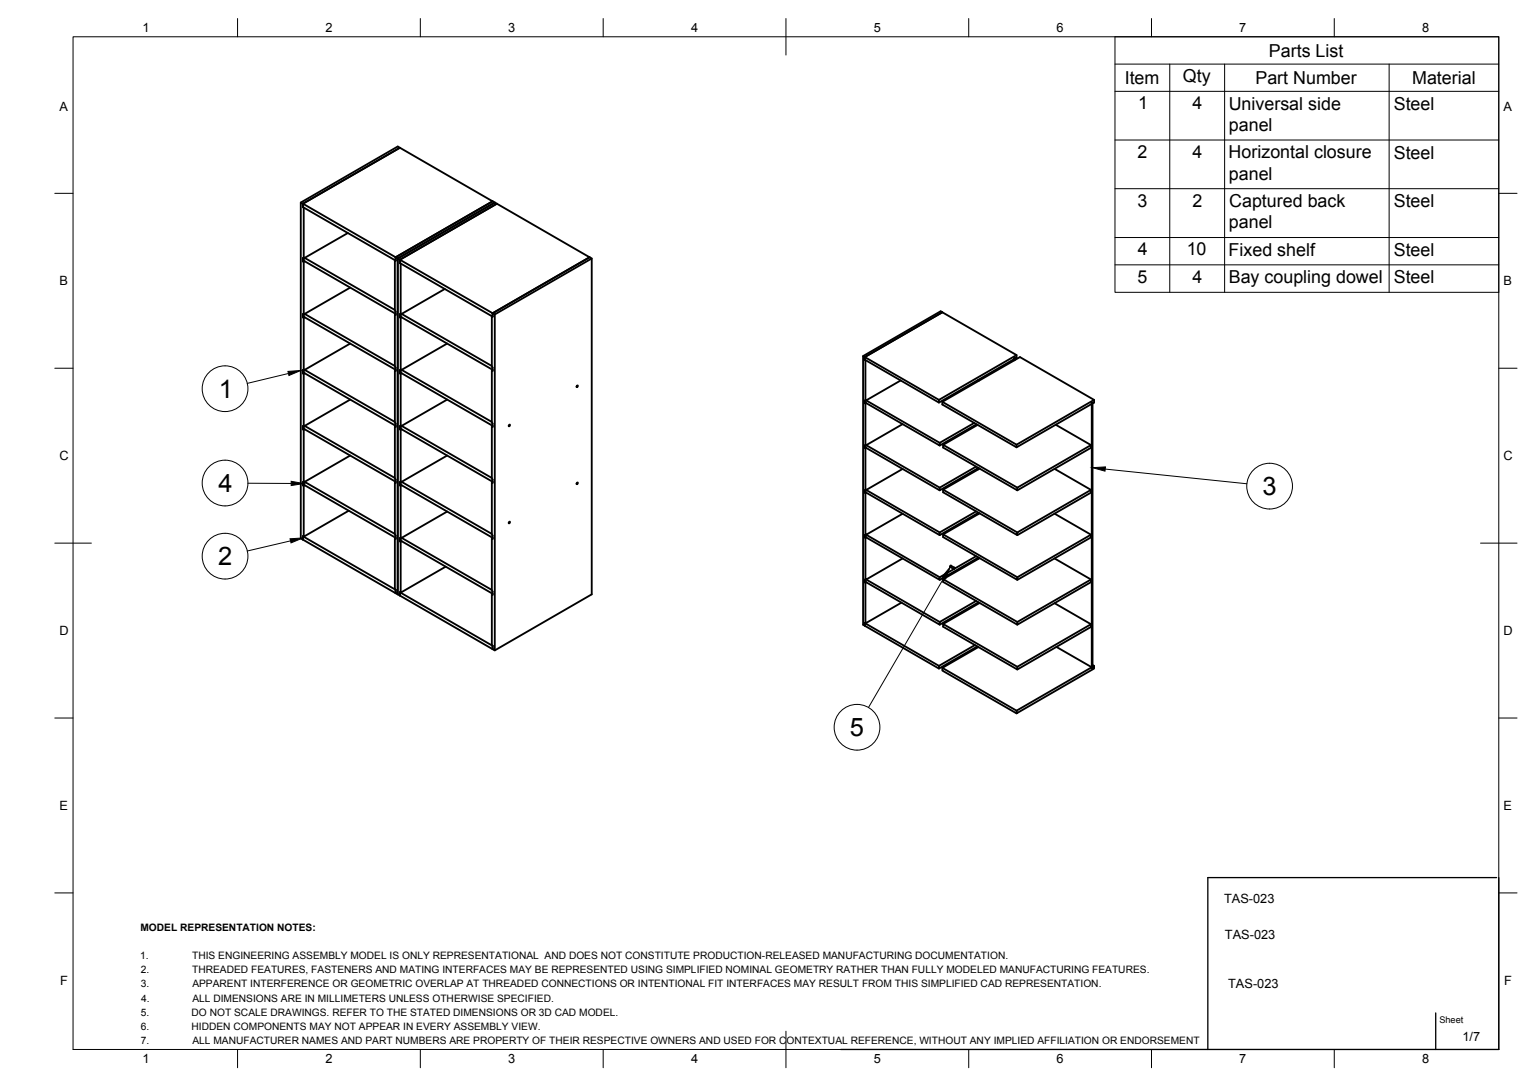
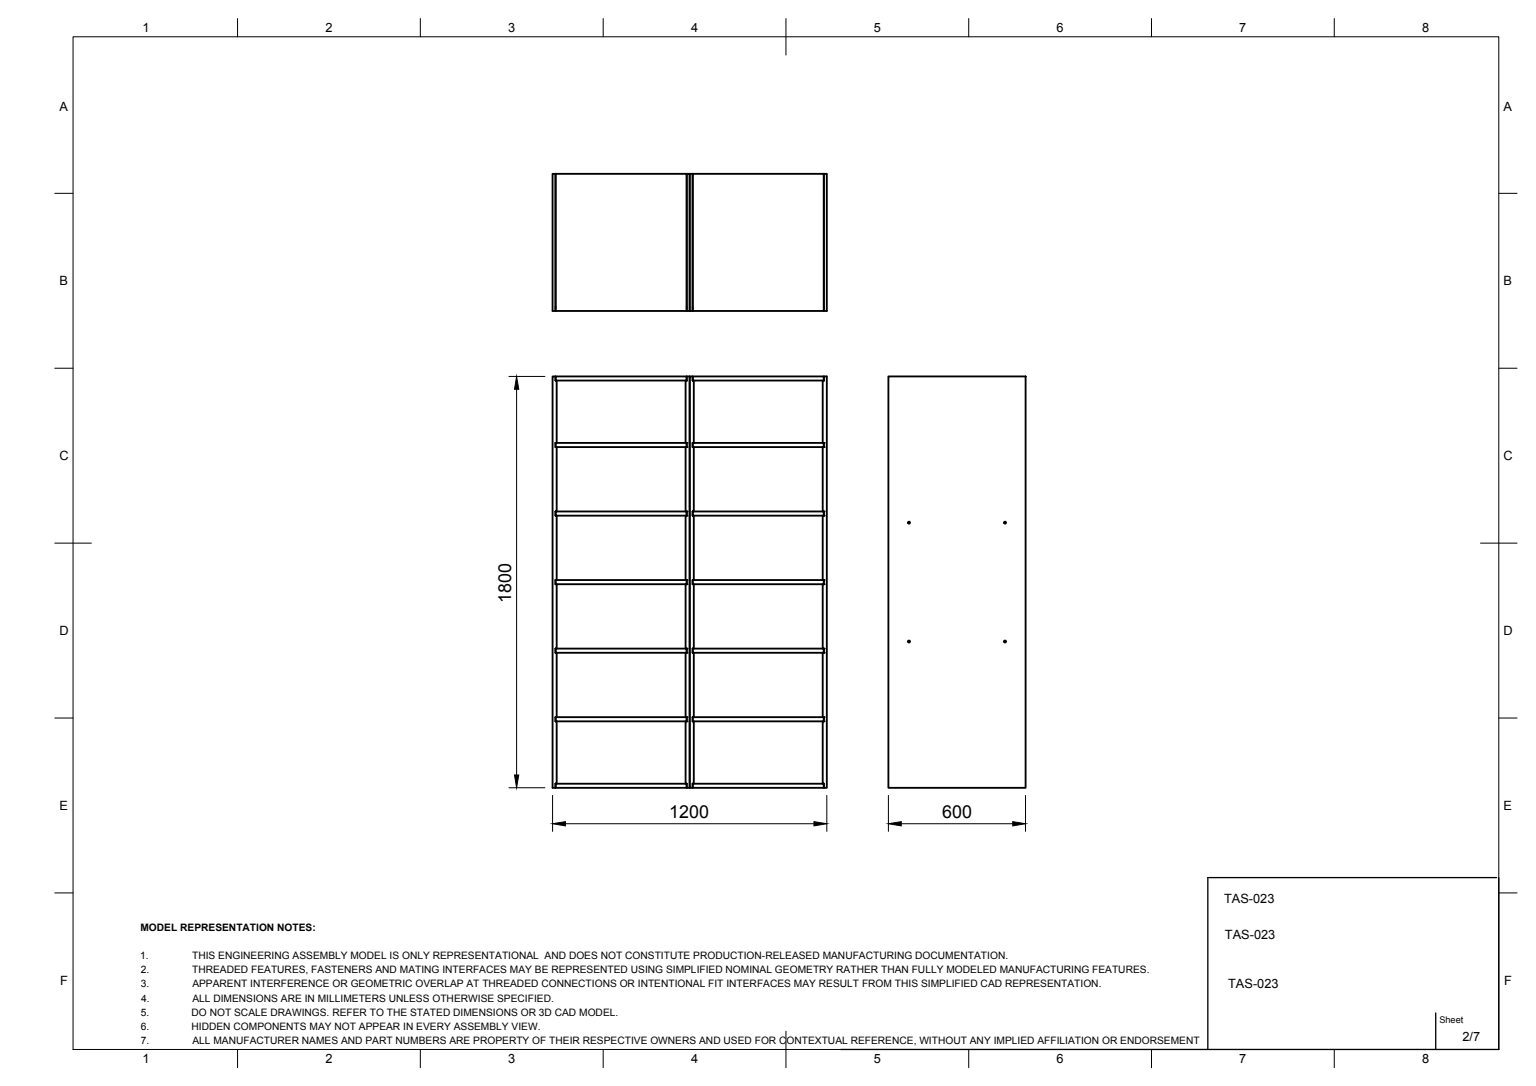
ISO-10303-21;
HEADER;
/* Generated by software containing ST-Developer
 * from STEP Tools, Inc. (www.steptools.com) 
 */

FILE_DESCRIPTION(
/* description */ (''),
/* implementation_level */ '2;1');

FILE_NAME(
/* name */ 'TAS-023.step',
/* time_stamp */ '2026-11-15T17:51:54-08:00',
/* author */ (''),
/* organization */ (''),
/* preprocessor_version */ 'ST-DEVELOPER v20.2',
/* originating_system */ 'Autodesk Translation Framework v15.17.0.0',
/* authorisation */ '');

FILE_SCHEMA (('AUTOMOTIVE_DESIGN { 1 0 10303 214 3 1 1 }'));
ENDSEC;

DATA;
#10=MECHANICAL_DESIGN_GEOMETRIC_PRESENTATION_REPRESENTATION('',(#117,#118,
#119,#120,#121),#2860);
#11=ITEM_DEFINED_TRANSFORMATION($,$,#1776,#1878);
#12=ITEM_DEFINED_TRANSFORMATION($,$,#1847,#1879);
#13=ITEM_DEFINED_TRANSFORMATION($,$,#1858,#1880);
#14=ITEM_DEFINED_TRANSFORMATION($,$,#1865,#1881);
#15=ITEM_DEFINED_TRANSFORMATION($,$,#1872,#1882);
#16=ITEM_DEFINED_TRANSFORMATION($,$,#1776,#1883);
#17=ITEM_DEFINED_TRANSFORMATION($,$,#1847,#1884);
#18=ITEM_DEFINED_TRANSFORMATION($,$,#1865,#1885);
#19=ITEM_DEFINED_TRANSFORMATION($,$,#1865,#1886);
#20=ITEM_DEFINED_TRANSFORMATION($,$,#1865,#1887);
#21=ITEM_DEFINED_TRANSFORMATION($,$,#1865,#1888);
#22=ITEM_DEFINED_TRANSFORMATION($,$,#1776,#1889);
#23=ITEM_DEFINED_TRANSFORMATION($,$,#1776,#1890);
#24=ITEM_DEFINED_TRANSFORMATION($,$,#1847,#1891);
#25=ITEM_DEFINED_TRANSFORMATION($,$,#1847,#1892);
#26=ITEM_DEFINED_TRANSFORMATION($,$,#1858,#1893);
#27=ITEM_DEFINED_TRANSFORMATION($,$,#1865,#1894);
#28=ITEM_DEFINED_TRANSFORMATION($,$,#1865,#1895);
#29=ITEM_DEFINED_TRANSFORMATION($,$,#1865,#1896);
#30=ITEM_DEFINED_TRANSFORMATION($,$,#1865,#1897);
#31=ITEM_DEFINED_TRANSFORMATION($,$,#1865,#1898);
#32=ITEM_DEFINED_TRANSFORMATION($,$,#1872,#1899);
#33=ITEM_DEFINED_TRANSFORMATION($,$,#1872,#1900);
#34=ITEM_DEFINED_TRANSFORMATION($,$,#1872,#1901);
#35=(
REPRESENTATION_RELATIONSHIP($,$,#2902,#2901)
REPRESENTATION_RELATIONSHIP_WITH_TRANSFORMATION(#11)
SHAPE_REPRESENTATION_RELATIONSHIP()
);
#36=(
REPRESENTATION_RELATIONSHIP($,$,#2903,#2901)
REPRESENTATION_RELATIONSHIP_WITH_TRANSFORMATION(#12)
SHAPE_REPRESENTATION_RELATIONSHIP()
);
#37=(
REPRESENTATION_RELATIONSHIP($,$,#2904,#2901)
REPRESENTATION_RELATIONSHIP_WITH_TRANSFORMATION(#13)
SHAPE_REPRESENTATION_RELATIONSHIP()
);
#38=(
REPRESENTATION_RELATIONSHIP($,$,#2905,#2901)
REPRESENTATION_RELATIONSHIP_WITH_TRANSFORMATION(#14)
SHAPE_REPRESENTATION_RELATIONSHIP()
);
#39=(
REPRESENTATION_RELATIONSHIP($,$,#2906,#2901)
REPRESENTATION_RELATIONSHIP_WITH_TRANSFORMATION(#15)
SHAPE_REPRESENTATION_RELATIONSHIP()
);
#40=(
REPRESENTATION_RELATIONSHIP($,$,#2902,#2901)
REPRESENTATION_RELATIONSHIP_WITH_TRANSFORMATION(#16)
SHAPE_REPRESENTATION_RELATIONSHIP()
);
#41=(
REPRESENTATION_RELATIONSHIP($,$,#2903,#2901)
REPRESENTATION_RELATIONSHIP_WITH_TRANSFORMATION(#17)
SHAPE_REPRESENTATION_RELATIONSHIP()
);
#42=(
REPRESENTATION_RELATIONSHIP($,$,#2905,#2901)
REPRESENTATION_RELATIONSHIP_WITH_TRANSFORMATION(#18)
SHAPE_REPRESENTATION_RELATIONSHIP()
);
#43=(
REPRESENTATION_RELATIONSHIP($,$,#2905,#2901)
REPRESENTATION_RELATIONSHIP_WITH_TRANSFORMATION(#19)
SHAPE_REPRESENTATION_RELATIONSHIP()
);
#44=(
REPRESENTATION_RELATIONSHIP($,$,#2905,#2901)
REPRESENTATION_RELATIONSHIP_WITH_TRANSFORMATION(#20)
SHAPE_REPRESENTATION_RELATIONSHIP()
);
#45=(
REPRESENTATION_RELATIONSHIP($,$,#2905,#2901)
REPRESENTATION_RELATIONSHIP_WITH_TRANSFORMATION(#21)
SHAPE_REPRESENTATION_RELATIONSHIP()
);
#46=(
REPRESENTATION_RELATIONSHIP($,$,#2902,#2901)
REPRESENTATION_RELATIONSHIP_WITH_TRANSFORMATION(#22)
SHAPE_REPRESENTATION_RELATIONSHIP()
);
#47=(
REPRESENTATION_RELATIONSHIP($,$,#2902,#2901)
REPRESENTATION_RELATIONSHIP_WITH_TRANSFORMATION(#23)
SHAPE_REPRESENTATION_RELATIONSHIP()
);
#48=(
REPRESENTATION_RELATIONSHIP($,$,#2903,#2901)
REPRESENTATION_RELATIONSHIP_WITH_TRANSFORMATION(#24)
SHAPE_REPRESENTATION_RELATIONSHIP()
);
#49=(
REPRESENTATION_RELATIONSHIP($,$,#2903,#2901)
REPRESENTATION_RELATIONSHIP_WITH_TRANSFORMATION(#25)
SHAPE_REPRESENTATION_RELATIONSHIP()
);
#50=(
REPRESENTATION_RELATIONSHIP($,$,#2904,#2901)
REPRESENTATION_RELATIONSHIP_WITH_TRANSFORMATION(#26)
SHAPE_REPRESENTATION_RELATIONSHIP()
);
#51=(
REPRESENTATION_RELATIONSHIP($,$,#2905,#2901)
REPRESENTATION_RELATIONSHIP_WITH_TRANSFORMATION(#27)
SHAPE_REPRESENTATION_RELATIONSHIP()
);
#52=(
REPRESENTATION_RELATIONSHIP($,$,#2905,#2901)
REPRESENTATION_RELATIONSHIP_WITH_TRANSFORMATION(#28)
SHAPE_REPRESENTATION_RELATIONSHIP()
);
#53=(
REPRESENTATION_RELATIONSHIP($,$,#2905,#2901)
REPRESENTATION_RELATIONSHIP_WITH_TRANSFORMATION(#29)
SHAPE_REPRESENTATION_RELATIONSHIP()
);
#54=(
REPRESENTATION_RELATIONSHIP($,$,#2905,#2901)
REPRESENTATION_RELATIONSHIP_WITH_TRANSFORMATION(#30)
SHAPE_REPRESENTATION_RELATIONSHIP()
);
#55=(
REPRESENTATION_RELATIONSHIP($,$,#2905,#2901)
REPRESENTATION_RELATIONSHIP_WITH_TRANSFORMATION(#31)
SHAPE_REPRESENTATION_RELATIONSHIP()
);
#56=(
REPRESENTATION_RELATIONSHIP($,$,#2906,#2901)
REPRESENTATION_RELATIONSHIP_WITH_TRANSFORMATION(#32)
SHAPE_REPRESENTATION_RELATIONSHIP()
);
#57=(
REPRESENTATION_RELATIONSHIP($,$,#2906,#2901)
REPRESENTATION_RELATIONSHIP_WITH_TRANSFORMATION(#33)
SHAPE_REPRESENTATION_RELATIONSHIP()
);
#58=(
REPRESENTATION_RELATIONSHIP($,$,#2906,#2901)
REPRESENTATION_RELATIONSHIP_WITH_TRANSFORMATION(#34)
SHAPE_REPRESENTATION_RELATIONSHIP()
);
#59=CONTEXT_DEPENDENT_SHAPE_REPRESENTATION(#35,#2877);
#60=CONTEXT_DEPENDENT_SHAPE_REPRESENTATION(#36,#2878);
#61=CONTEXT_DEPENDENT_SHAPE_REPRESENTATION(#37,#2879);
#62=CONTEXT_DEPENDENT_SHAPE_REPRESENTATION(#38,#2880);
#63=CONTEXT_DEPENDENT_SHAPE_REPRESENTATION(#39,#2881);
#64=CONTEXT_DEPENDENT_SHAPE_REPRESENTATION(#40,#2882);
#65=CONTEXT_DEPENDENT_SHAPE_REPRESENTATION(#41,#2883);
#66=CONTEXT_DEPENDENT_SHAPE_REPRESENTATION(#42,#2884);
#67=CONTEXT_DEPENDENT_SHAPE_REPRESENTATION(#43,#2885);
#68=CONTEXT_DEPENDENT_SHAPE_REPRESENTATION(#44,#2886);
#69=CONTEXT_DEPENDENT_SHAPE_REPRESENTATION(#45,#2887);
#70=CONTEXT_DEPENDENT_SHAPE_REPRESENTATION(#46,#2888);
#71=CONTEXT_DEPENDENT_SHAPE_REPRESENTATION(#47,#2889);
#72=CONTEXT_DEPENDENT_SHAPE_REPRESENTATION(#48,#2890);
#73=CONTEXT_DEPENDENT_SHAPE_REPRESENTATION(#49,#2891);
#74=CONTEXT_DEPENDENT_SHAPE_REPRESENTATION(#50,#2892);
#75=CONTEXT_DEPENDENT_SHAPE_REPRESENTATION(#51,#2893);
#76=CONTEXT_DEPENDENT_SHAPE_REPRESENTATION(#52,#2894);
#77=CONTEXT_DEPENDENT_SHAPE_REPRESENTATION(#53,#2895);
#78=CONTEXT_DEPENDENT_SHAPE_REPRESENTATION(#54,#2896);
#79=CONTEXT_DEPENDENT_SHAPE_REPRESENTATION(#55,#2897);
#80=CONTEXT_DEPENDENT_SHAPE_REPRESENTATION(#56,#2898);
#81=CONTEXT_DEPENDENT_SHAPE_REPRESENTATION(#57,#2899);
#82=CONTEXT_DEPENDENT_SHAPE_REPRESENTATION(#58,#2900);
#83=NEXT_ASSEMBLY_USAGE_OCCURRENCE('Universal side panel:1',
'Universal side panel:1','Universal side panel:1',#2908,#2909,
'Universal side panel:1');
#84=NEXT_ASSEMBLY_USAGE_OCCURRENCE('Horizontal closure panel:1',
'Horizontal closure panel:1','Horizontal closure panel:1',#2908,#2910,
'Horizontal closure panel:1');
#85=NEXT_ASSEMBLY_USAGE_OCCURRENCE('Captured back panel:1',
'Captured back panel:1','Captured back panel:1',#2908,#2911,
'Captured back panel:1');
#86=NEXT_ASSEMBLY_USAGE_OCCURRENCE('Fixed shelf:1','Fixed shelf:1',
'Fixed shelf:1',#2908,#2912,'Fixed shelf:1');
#87=NEXT_ASSEMBLY_USAGE_OCCURRENCE('Bay coupling dowel:1',
'Bay coupling dowel:1','Bay coupling dowel:1',#2908,#2913,
'Bay coupling dowel:1');
#88=NEXT_ASSEMBLY_USAGE_OCCURRENCE('Universal side panel:2',
'Universal side panel:2','Universal side panel:2',#2908,#2909,
'Universal side panel:2');
#89=NEXT_ASSEMBLY_USAGE_OCCURRENCE('Horizontal closure panel:2',
'Horizontal closure panel:2','Horizontal closure panel:2',#2908,#2910,
'Horizontal closure panel:2');
#90=NEXT_ASSEMBLY_USAGE_OCCURRENCE('Fixed shelf:2','Fixed shelf:2',
'Fixed shelf:2',#2908,#2912,'Fixed shelf:2');
#91=NEXT_ASSEMBLY_USAGE_OCCURRENCE('Fixed shelf:3','Fixed shelf:3',
'Fixed shelf:3',#2908,#2912,'Fixed shelf:3');
#92=NEXT_ASSEMBLY_USAGE_OCCURRENCE('Fixed shelf:4','Fixed shelf:4',
'Fixed shelf:4',#2908,#2912,'Fixed shelf:4');
#93=NEXT_ASSEMBLY_USAGE_OCCURRENCE('Fixed shelf:5','Fixed shelf:5',
'Fixed shelf:5',#2908,#2912,'Fixed shelf:5');
#94=NEXT_ASSEMBLY_USAGE_OCCURRENCE('Universal side panel:3',
'Universal side panel:3','Universal side panel:3',#2908,#2909,
'Universal side panel:3');
#95=NEXT_ASSEMBLY_USAGE_OCCURRENCE('Universal side panel:4',
'Universal side panel:4','Universal side panel:4',#2908,#2909,
'Universal side panel:4');
#96=NEXT_ASSEMBLY_USAGE_OCCURRENCE('Horizontal closure panel:3',
'Horizontal closure panel:3','Horizontal closure panel:3',#2908,#2910,
'Horizontal closure panel:3');
#97=NEXT_ASSEMBLY_USAGE_OCCURRENCE('Horizontal closure panel:4',
'Horizontal closure panel:4','Horizontal closure panel:4',#2908,#2910,
'Horizontal closure panel:4');
#98=NEXT_ASSEMBLY_USAGE_OCCURRENCE('Captured back panel:2',
'Captured back panel:2','Captured back panel:2',#2908,#2911,
'Captured back panel:2');
#99=NEXT_ASSEMBLY_USAGE_OCCURRENCE('Fixed shelf:6','Fixed shelf:6',
'Fixed shelf:6',#2908,#2912,'Fixed shelf:6');
#100=NEXT_ASSEMBLY_USAGE_OCCURRENCE('Fixed shelf:7','Fixed shelf:7',
'Fixed shelf:7',#2908,#2912,'Fixed shelf:7');
#101=NEXT_ASSEMBLY_USAGE_OCCURRENCE('Fixed shelf:8','Fixed shelf:8',
'Fixed shelf:8',#2908,#2912,'Fixed shelf:8');
#102=NEXT_ASSEMBLY_USAGE_OCCURRENCE('Fixed shelf:9','Fixed shelf:9',
'Fixed shelf:9',#2908,#2912,'Fixed shelf:9');
#103=NEXT_ASSEMBLY_USAGE_OCCURRENCE('Fixed shelf:10','Fixed shelf:10',
'Fixed shelf:10',#2908,#2912,'Fixed shelf:10');
#104=NEXT_ASSEMBLY_USAGE_OCCURRENCE('Bay coupling dowel:2',
'Bay coupling dowel:2','Bay coupling dowel:2',#2908,#2913,
'Bay coupling dowel:2');
#105=NEXT_ASSEMBLY_USAGE_OCCURRENCE('Bay coupling dowel:3',
'Bay coupling dowel:3','Bay coupling dowel:3',#2908,#2913,
'Bay coupling dowel:3');
#106=NEXT_ASSEMBLY_USAGE_OCCURRENCE('Bay coupling dowel:4',
'Bay coupling dowel:4','Bay coupling dowel:4',#2908,#2913,
'Bay coupling dowel:4');
#107=SHAPE_REPRESENTATION_RELATIONSHIP('SRR','None',#2902,#112);
#108=SHAPE_REPRESENTATION_RELATIONSHIP('SRR','None',#2903,#113);
#109=SHAPE_REPRESENTATION_RELATIONSHIP('SRR','None',#2904,#114);
#110=SHAPE_REPRESENTATION_RELATIONSHIP('SRR','None',#2905,#115);
#111=SHAPE_REPRESENTATION_RELATIONSHIP('SRR','None',#2906,#116);
#112=ADVANCED_BREP_SHAPE_REPRESENTATION('',(#122),#2855);
#113=ADVANCED_BREP_SHAPE_REPRESENTATION('',(#123),#2856);
#114=ADVANCED_BREP_SHAPE_REPRESENTATION('',(#124),#2857);
#115=ADVANCED_BREP_SHAPE_REPRESENTATION('',(#125),#2858);
#116=ADVANCED_BREP_SHAPE_REPRESENTATION('',(#126),#2859);
#117=STYLED_ITEM('',(#2936),#122);
#118=STYLED_ITEM('',(#2937),#123);
#119=STYLED_ITEM('',(#2938),#124);
#120=STYLED_ITEM('',(#2939),#125);
#121=STYLED_ITEM('',(#2940),#126);
#122=MANIFOLD_SOLID_BREP('Body1',#1714);
#123=MANIFOLD_SOLID_BREP('Body1',#1715);
#124=MANIFOLD_SOLID_BREP('Body1',#1716);
#125=MANIFOLD_SOLID_BREP('Body1',#1717);
#126=MANIFOLD_SOLID_BREP('Body1',#1718);
#127=FACE_BOUND('',#361,.T.);
#128=FACE_BOUND('',#362,.T.);
#129=FACE_BOUND('',#363,.T.);
#130=FACE_BOUND('',#364,.T.);
#131=PLANE('',#1780);
#132=PLANE('',#1784);
#133=PLANE('',#1788);
#134=PLANE('',#1792);
#135=PLANE('',#1793);
#136=PLANE('',#1794);
#137=PLANE('',#1795);
#138=PLANE('',#1796);
#139=PLANE('',#1797);
#140=PLANE('',#1798);
#141=PLANE('',#1799);
#142=PLANE('',#1800);
#143=PLANE('',#1801);
#144=PLANE('',#1802);
#145=PLANE('',#1803);
#146=PLANE('',#1804);
#147=PLANE('',#1805);
#148=PLANE('',#1806);
#149=PLANE('',#1807);
#150=PLANE('',#1808);
#151=PLANE('',#1809);
#152=PLANE('',#1810);
#153=PLANE('',#1811);
#154=PLANE('',#1812);
#155=PLANE('',#1813);
#156=PLANE('',#1814);
#157=PLANE('',#1815);
#158=PLANE('',#1816);
#159=PLANE('',#1817);
#160=PLANE('',#1818);
#161=PLANE('',#1819);
#162=PLANE('',#1820);
#163=PLANE('',#1821);
#164=PLANE('',#1822);
#165=PLANE('',#1823);
#166=PLANE('',#1824);
#167=PLANE('',#1825);
#168=PLANE('',#1826);
#169=PLANE('',#1827);
#170=PLANE('',#1828);
#171=PLANE('',#1829);
#172=PLANE('',#1830);
#173=PLANE('',#1831);
#174=PLANE('',#1832);
#175=PLANE('',#1833);
#176=PLANE('',#1834);
#177=PLANE('',#1835);
#178=PLANE('',#1836);
#179=PLANE('',#1837);
#180=PLANE('',#1838);
#181=PLANE('',#1839);
#182=PLANE('',#1840);
#183=PLANE('',#1841);
#184=PLANE('',#1842);
#185=PLANE('',#1843);
#186=PLANE('',#1844);
#187=PLANE('',#1845);
#188=PLANE('',#1846);
#189=PLANE('',#1848);
#190=PLANE('',#1849);
#191=PLANE('',#1850);
#192=PLANE('',#1851);
#193=PLANE('',#1852);
#194=PLANE('',#1853);
#195=PLANE('',#1854);
#196=PLANE('',#1855);
#197=PLANE('',#1856);
#198=PLANE('',#1857);
#199=PLANE('',#1859);
#200=PLANE('',#1860);
#201=PLANE('',#1861);
#202=PLANE('',#1862);
#203=PLANE('',#1863);
#204=PLANE('',#1864);
#205=PLANE('',#1866);
#206=PLANE('',#1867);
#207=PLANE('',#1868);
#208=PLANE('',#1869);
#209=PLANE('',#1870);
#210=PLANE('',#1871);
#211=PLANE('',#1876);
#212=PLANE('',#1877);
#213=FACE_OUTER_BOUND('',#300,.T.);
#214=FACE_OUTER_BOUND('',#301,.T.);
#215=FACE_OUTER_BOUND('',#302,.T.);
#216=FACE_OUTER_BOUND('',#303,.T.);
#217=FACE_OUTER_BOUND('',#304,.T.);
#218=FACE_OUTER_BOUND('',#305,.T.);
#219=FACE_OUTER_BOUND('',#306,.T.);
#220=FACE_OUTER_BOUND('',#307,.T.);
#221=FACE_OUTER_BOUND('',#308,.T.);
#222=FACE_OUTER_BOUND('',#309,.T.);
#223=FACE_OUTER_BOUND('',#310,.T.);
#224=FACE_OUTER_BOUND('',#311,.T.);
#225=FACE_OUTER_BOUND('',#312,.T.);
#226=FACE_OUTER_BOUND('',#313,.T.);
#227=FACE_OUTER_BOUND('',#314,.T.);
#228=FACE_OUTER_BOUND('',#315,.T.);
#229=FACE_OUTER_BOUND('',#316,.T.);
#230=FACE_OUTER_BOUND('',#317,.T.);
#231=FACE_OUTER_BOUND('',#318,.T.);
#232=FACE_OUTER_BOUND('',#319,.T.);
#233=FACE_OUTER_BOUND('',#320,.T.);
#234=FACE_OUTER_BOUND('',#321,.T.);
#235=FACE_OUTER_BOUND('',#322,.T.);
#236=FACE_OUTER_BOUND('',#323,.T.);
#237=FACE_OUTER_BOUND('',#324,.T.);
#238=FACE_OUTER_BOUND('',#325,.T.);
#239=FACE_OUTER_BOUND('',#326,.T.);
#240=FACE_OUTER_BOUND('',#327,.T.);
#241=FACE_OUTER_BOUND('',#328,.T.);
#242=FACE_OUTER_BOUND('',#329,.T.);
#243=FACE_OUTER_BOUND('',#330,.T.);
#244=FACE_OUTER_BOUND('',#331,.T.);
#245=FACE_OUTER_BOUND('',#332,.T.);
#246=FACE_OUTER_BOUND('',#333,.T.);
#247=FACE_OUTER_BOUND('',#334,.T.);
#248=FACE_OUTER_BOUND('',#335,.T.);
#249=FACE_OUTER_BOUND('',#336,.T.);
#250=FACE_OUTER_BOUND('',#337,.T.);
#251=FACE_OUTER_BOUND('',#338,.T.);
#252=FACE_OUTER_BOUND('',#339,.T.);
#253=FACE_OUTER_BOUND('',#340,.T.);
#254=FACE_OUTER_BOUND('',#341,.T.);
#255=FACE_OUTER_BOUND('',#342,.T.);
#256=FACE_OUTER_BOUND('',#343,.T.);
#257=FACE_OUTER_BOUND('',#344,.T.);
#258=FACE_OUTER_BOUND('',#345,.T.);
#259=FACE_OUTER_BOUND('',#346,.T.);
#260=FACE_OUTER_BOUND('',#347,.T.);
#261=FACE_OUTER_BOUND('',#348,.T.);
#262=FACE_OUTER_BOUND('',#349,.T.);
#263=FACE_OUTER_BOUND('',#350,.T.);
#264=FACE_OUTER_BOUND('',#351,.T.);
#265=FACE_OUTER_BOUND('',#352,.T.);
#266=FACE_OUTER_BOUND('',#353,.T.);
#267=FACE_OUTER_BOUND('',#354,.T.);
#268=FACE_OUTER_BOUND('',#355,.T.);
#269=FACE_OUTER_BOUND('',#356,.T.);
#270=FACE_OUTER_BOUND('',#357,.T.);
#271=FACE_OUTER_BOUND('',#358,.T.);
#272=FACE_OUTER_BOUND('',#359,.T.);
#273=FACE_OUTER_BOUND('',#360,.T.);
#274=FACE_OUTER_BOUND('',#365,.T.);
#275=FACE_OUTER_BOUND('',#366,.T.);
#276=FACE_OUTER_BOUND('',#367,.T.);
#277=FACE_OUTER_BOUND('',#368,.T.);
#278=FACE_OUTER_BOUND('',#369,.T.);
#279=FACE_OUTER_BOUND('',#370,.T.);
#280=FACE_OUTER_BOUND('',#371,.T.);
#281=FACE_OUTER_BOUND('',#372,.T.);
#282=FACE_OUTER_BOUND('',#373,.T.);
#283=FACE_OUTER_BOUND('',#374,.T.);
#284=FACE_OUTER_BOUND('',#375,.T.);
#285=FACE_OUTER_BOUND('',#376,.T.);
#286=FACE_OUTER_BOUND('',#377,.T.);
#287=FACE_OUTER_BOUND('',#378,.T.);
#288=FACE_OUTER_BOUND('',#379,.T.);
#289=FACE_OUTER_BOUND('',#380,.T.);
#290=FACE_OUTER_BOUND('',#381,.T.);
#291=FACE_OUTER_BOUND('',#382,.T.);
#292=FACE_OUTER_BOUND('',#383,.T.);
#293=FACE_OUTER_BOUND('',#384,.T.);
#294=FACE_OUTER_BOUND('',#385,.T.);
#295=FACE_OUTER_BOUND('',#386,.T.);
#296=FACE_OUTER_BOUND('',#387,.T.);
#297=FACE_OUTER_BOUND('',#388,.T.);
#298=FACE_OUTER_BOUND('',#389,.T.);
#299=FACE_OUTER_BOUND('',#390,.T.);
#300=EDGE_LOOP('',(#1184,#1185,#1186,#1187));
#301=EDGE_LOOP('',(#1188));
#302=EDGE_LOOP('',(#1189,#1190,#1191,#1192));
#303=EDGE_LOOP('',(#1193));
#304=EDGE_LOOP('',(#1194,#1195,#1196,#1197));
#305=EDGE_LOOP('',(#1198));
#306=EDGE_LOOP('',(#1199,#1200,#1201,#1202));
#307=EDGE_LOOP('',(#1203));
#308=EDGE_LOOP('',(#1204,#1205,#1206,#1207));
#309=EDGE_LOOP('',(#1208,#1209,#1210,#1211));
#310=EDGE_LOOP('',(#1212,#1213,#1214,#1215));
#311=EDGE_LOOP('',(#1216,#1217,#1218,#1219));
#312=EDGE_LOOP('',(#1220,#1221,#1222,#1223));
#313=EDGE_LOOP('',(#1224,#1225,#1226,#1227));
#314=EDGE_LOOP('',(#1228,#1229,#1230,#1231));
#315=EDGE_LOOP('',(#1232,#1233,#1234,#1235));
#316=EDGE_LOOP('',(#1236,#1237,#1238,#1239));
#317=EDGE_LOOP('',(#1240,#1241,#1242,#1243));
#318=EDGE_LOOP('',(#1244,#1245,#1246,#1247));
#319=EDGE_LOOP('',(#1248,#1249,#1250,#1251));
#320=EDGE_LOOP('',(#1252,#1253,#1254,#1255,#1256,#1257,#1258,#1259,#1260,
#1261,#1262,#1263,#1264,#1265,#1266,#1267,#1268,#1269,#1270,#1271,#1272,
#1273,#1274,#1275,#1276,#1277,#1278,#1279,#1280,#1281,#1282,#1283,#1284,
#1285,#1286,#1287,#1288,#1289,#1290,#1291,#1292,#1293,#1294,#1295,#1296,
#1297,#1298,#1299,#1300,#1301,#1302,#1303));
#321=EDGE_LOOP('',(#1304,#1305,#1306,#1307));
#322=EDGE_LOOP('',(#1308,#1309,#1310,#1311));
#323=EDGE_LOOP('',(#1312,#1313,#1314,#1315));
#324=EDGE_LOOP('',(#1316,#1317,#1318,#1319));
#325=EDGE_LOOP('',(#1320,#1321,#1322,#1323));
#326=EDGE_LOOP('',(#1324,#1325,#1326,#1327));
#327=EDGE_LOOP('',(#1328,#1329,#1330,#1331));
#328=EDGE_LOOP('',(#1332,#1333,#1334,#1335));
#329=EDGE_LOOP('',(#1336,#1337,#1338,#1339));
#330=EDGE_LOOP('',(#1340,#1341,#1342,#1343));
#331=EDGE_LOOP('',(#1344,#1345,#1346,#1347));
#332=EDGE_LOOP('',(#1348,#1349,#1350,#1351));
#333=EDGE_LOOP('',(#1352,#1353,#1354,#1355));
#334=EDGE_LOOP('',(#1356,#1357,#1358,#1359));
#335=EDGE_LOOP('',(#1360,#1361,#1362,#1363));
#336=EDGE_LOOP('',(#1364,#1365,#1366,#1367));
#337=EDGE_LOOP('',(#1368,#1369,#1370,#1371));
#338=EDGE_LOOP('',(#1372,#1373,#1374,#1375));
#339=EDGE_LOOP('',(#1376,#1377,#1378,#1379));
#340=EDGE_LOOP('',(#1380,#1381,#1382,#1383));
#341=EDGE_LOOP('',(#1384,#1385,#1386,#1387));
#342=EDGE_LOOP('',(#1388,#1389,#1390,#1391));
#343=EDGE_LOOP('',(#1392,#1393,#1394,#1395));
#344=EDGE_LOOP('',(#1396,#1397,#1398,#1399));
#345=EDGE_LOOP('',(#1400,#1401,#1402,#1403));
#346=EDGE_LOOP('',(#1404,#1405,#1406,#1407));
#347=EDGE_LOOP('',(#1408,#1409,#1410,#1411));
#348=EDGE_LOOP('',(#1412,#1413,#1414,#1415));
#349=EDGE_LOOP('',(#1416,#1417,#1418,#1419));
#350=EDGE_LOOP('',(#1420,#1421,#1422,#1423));
#351=EDGE_LOOP('',(#1424,#1425,#1426,#1427));
#352=EDGE_LOOP('',(#1428,#1429,#1430,#1431));
#353=EDGE_LOOP('',(#1432,#1433,#1434,#1435));
#354=EDGE_LOOP('',(#1436,#1437,#1438,#1439));
#355=EDGE_LOOP('',(#1440,#1441,#1442,#1443));
#356=EDGE_LOOP('',(#1444,#1445,#1446,#1447));
#357=EDGE_LOOP('',(#1448,#1449,#1450,#1451,#1452,#1453,#1454,#1455,#1456,
#1457,#1458,#1459,#1460,#1461,#1462,#1463,#1464,#1465,#1466,#1467,#1468,
#1469,#1470,#1471,#1472,#1473,#1474,#1475));
#358=EDGE_LOOP('',(#1476,#1477,#1478,#1479));
#359=EDGE_LOOP('',(#1480,#1481,#1482,#1483,#1484,#1485,#1486,#1487,#1488,
#1489,#1490,#1491,#1492,#1493,#1494,#1495,#1496,#1497,#1498,#1499,#1500,
#1501,#1502,#1503,#1504,#1505,#1506,#1507));
#360=EDGE_LOOP('',(#1508,#1509,#1510,#1511));
#361=EDGE_LOOP('',(#1512));
#362=EDGE_LOOP('',(#1513));
#363=EDGE_LOOP('',(#1514));
#364=EDGE_LOOP('',(#1515));
#365=EDGE_LOOP('',(#1516,#1517,#1518,#1519));
#366=EDGE_LOOP('',(#1520,#1521,#1522,#1523));
#367=EDGE_LOOP('',(#1524,#1525,#1526,#1527));
#368=EDGE_LOOP('',(#1528,#1529,#1530,#1531));
#369=EDGE_LOOP('',(#1532,#1533,#1534,#1535,#1536,#1537,#1538,#1539));
#370=EDGE_LOOP('',(#1540,#1541,#1542,#1543));
#371=EDGE_LOOP('',(#1544,#1545,#1546,#1547));
#372=EDGE_LOOP('',(#1548,#1549,#1550,#1551));
#373=EDGE_LOOP('',(#1552,#1553,#1554,#1555,#1556,#1557,#1558,#1559));
#374=EDGE_LOOP('',(#1560,#1561,#1562,#1563));
#375=EDGE_LOOP('',(#1564,#1565,#1566,#1567));
#376=EDGE_LOOP('',(#1568,#1569,#1570,#1571));
#377=EDGE_LOOP('',(#1572,#1573,#1574,#1575));
#378=EDGE_LOOP('',(#1576,#1577,#1578,#1579));
#379=EDGE_LOOP('',(#1580,#1581,#1582,#1583));
#380=EDGE_LOOP('',(#1584,#1585,#1586,#1587));
#381=EDGE_LOOP('',(#1588,#1589,#1590,#1591));
#382=EDGE_LOOP('',(#1592,#1593,#1594,#1595));
#383=EDGE_LOOP('',(#1596,#1597,#1598,#1599));
#384=EDGE_LOOP('',(#1600,#1601,#1602,#1603));
#385=EDGE_LOOP('',(#1604,#1605,#1606,#1607));
#386=EDGE_LOOP('',(#1608,#1609,#1610,#1611));
#387=EDGE_LOOP('',(#1612,#1613,#1614,#1615));
#388=EDGE_LOOP('',(#1616,#1617,#1618,#1619));
#389=EDGE_LOOP('',(#1620));
#390=EDGE_LOOP('',(#1621));
#391=LINE('',#2371,#600);
#392=LINE('',#2378,#601);
#393=LINE('',#2385,#602);
#394=LINE('',#2392,#603);
#395=LINE('',#2398,#604);
#396=LINE('',#2400,#605);
#397=LINE('',#2402,#606);
#398=LINE('',#2403,#607);
#399=LINE('',#2407,#608);
#400=LINE('',#2409,#609);
#401=LINE('',#2411,#610);
#402=LINE('',#2412,#611);
#403=LINE('',#2416,#612);
#404=LINE('',#2418,#613);
#405=LINE('',#2420,#614);
#406=LINE('',#2421,#615);
#407=LINE('',#2425,#616);
#408=LINE('',#2427,#617);
#409=LINE('',#2429,#618);
#410=LINE('',#2430,#619);
#411=LINE('',#2434,#620);
#412=LINE('',#2436,#621);
#413=LINE('',#2438,#622);
#414=LINE('',#2439,#623);
#415=LINE('',#2443,#624);
#416=LINE('',#2445,#625);
#417=LINE('',#2447,#626);
#418=LINE('',#2448,#627);
#419=LINE('',#2452,#628);
#420=LINE('',#2454,#629);
#421=LINE('',#2456,#630);
#422=LINE('',#2457,#631);
#423=LINE('',#2461,#632);
#424=LINE('',#2463,#633);
#425=LINE('',#2465,#634);
#426=LINE('',#2466,#635);
#427=LINE('',#2470,#636);
#428=LINE('',#2472,#637);
#429=LINE('',#2474,#638);
#430=LINE('',#2475,#639);
#431=LINE('',#2479,#640);
#432=LINE('',#2481,#641);
#433=LINE('',#2483,#642);
#434=LINE('',#2484,#643);
#435=LINE('',#2488,#644);
#436=LINE('',#2490,#645);
#437=LINE('',#2492,#646);
#438=LINE('',#2493,#647);
#439=LINE('',#2497,#648);
#440=LINE('',#2499,#649);
#441=LINE('',#2501,#650);
#442=LINE('',#2502,#651);
#443=LINE('',#2505,#652);
#444=LINE('',#2507,#653);
#445=LINE('',#2509,#654);
#446=LINE('',#2511,#655);
#447=LINE('',#2512,#656);
#448=LINE('',#2514,#657);
#449=LINE('',#2516,#658);
#450=LINE('',#2517,#659);
#451=LINE('',#2519,#660);
#452=LINE('',#2521,#661);
#453=LINE('',#2522,#662);
#454=LINE('',#2524,#663);
#455=LINE('',#2526,#664);
#456=LINE('',#2527,#665);
#457=LINE('',#2529,#666);
#458=LINE('',#2531,#667);
#459=LINE('',#2532,#668);
#460=LINE('',#2534,#669);
#461=LINE('',#2536,#670);
#462=LINE('',#2537,#671);
#463=LINE('',#2539,#672);
#464=LINE('',#2541,#673);
#465=LINE('',#2543,#674);
#466=LINE('',#2545,#675);
#467=LINE('',#2546,#676);
#468=LINE('',#2548,#677);
#469=LINE('',#2550,#678);
#470=LINE('',#2551,#679);
#471=LINE('',#2553,#680);
#472=LINE('',#2555,#681);
#473=LINE('',#2556,#682);
#474=LINE('',#2558,#683);
#475=LINE('',#2560,#684);
#476=LINE('',#2561,#685);
#477=LINE('',#2563,#686);
#478=LINE('',#2565,#687);
#479=LINE('',#2566,#688);
#480=LINE('',#2568,#689);
#481=LINE('',#2570,#690);
#482=LINE('',#2571,#691);
#483=LINE('',#2574,#692);
#484=LINE('',#2575,#693);
#485=LINE('',#2578,#694);
#486=LINE('',#2579,#695);
#487=LINE('',#2582,#696);
#488=LINE('',#2583,#697);
#489=LINE('',#2586,#698);
#490=LINE('',#2587,#699);
#491=LINE('',#2589,#700);
#492=LINE('',#2591,#701);
#493=LINE('',#2594,#702);
#494=LINE('',#2595,#703);
#495=LINE('',#2598,#704);
#496=LINE('',#2599,#705);
#497=LINE('',#2602,#706);
#498=LINE('',#2603,#707);
#499=LINE('',#2606,#708);
#500=LINE('',#2607,#709);
#501=LINE('',#2609,#710);
#502=LINE('',#2611,#711);
#503=LINE('',#2614,#712);
#504=LINE('',#2615,#713);
#505=LINE('',#2618,#714);
#506=LINE('',#2619,#715);
#507=LINE('',#2622,#716);
#508=LINE('',#2623,#717);
#509=LINE('',#2626,#718);
#510=LINE('',#2627,#719);
#511=LINE('',#2629,#720);
#512=LINE('',#2631,#721);
#513=LINE('',#2634,#722);
#514=LINE('',#2635,#723);
#515=LINE('',#2638,#724);
#516=LINE('',#2639,#725);
#517=LINE('',#2642,#726);
#518=LINE('',#2643,#727);
#519=LINE('',#2646,#728);
#520=LINE('',#2647,#729);
#521=LINE('',#2649,#730);
#522=LINE('',#2651,#731);
#523=LINE('',#2654,#732);
#524=LINE('',#2655,#733);
#525=LINE('',#2658,#734);
#526=LINE('',#2659,#735);
#527=LINE('',#2662,#736);
#528=LINE('',#2663,#737);
#529=LINE('',#2666,#738);
#530=LINE('',#2667,#739);
#531=LINE('',#2669,#740);
#532=LINE('',#2671,#741);
#533=LINE('',#2674,#742);
#534=LINE('',#2675,#743);
#535=LINE('',#2678,#744);
#536=LINE('',#2679,#745);
#537=LINE('',#2682,#746);
#538=LINE('',#2683,#747);
#539=LINE('',#2686,#748);
#540=LINE('',#2687,#749);
#541=LINE('',#2689,#750);
#542=LINE('',#2691,#751);
#543=LINE('',#2694,#752);
#544=LINE('',#2696,#753);
#545=LINE('',#2697,#754);
#546=LINE('',#2700,#755);
#547=LINE('',#2701,#756);
#548=LINE('',#2704,#757);
#549=LINE('',#2705,#758);
#550=LINE('',#2707,#759);
#551=LINE('',#2713,#760);
#552=LINE('',#2715,#761);
#553=LINE('',#2717,#762);
#554=LINE('',#2718,#763);
#555=LINE('',#2722,#764);
#556=LINE('',#2724,#765);
#557=LINE('',#2726,#766);
#558=LINE('',#2727,#767);
#559=LINE('',#2729,#768);
#560=LINE('',#2730,#769);
#561=LINE('',#2733,#770);
#562=LINE('',#2735,#771);
#563=LINE('',#2737,#772);
#564=LINE('',#2739,#773);
#565=LINE('',#2740,#774);
#566=LINE('',#2743,#775);
#567=LINE('',#2744,#776);
#568=LINE('',#2747,#777);
#569=LINE('',#2749,#778);
#570=LINE('',#2750,#779);
#571=LINE('',#2753,#780);
#572=LINE('',#2754,#781);
#573=LINE('',#2756,#782);
#574=LINE('',#2757,#783);
#575=LINE('',#2764,#784);
#576=LINE('',#2766,#785);
#577=LINE('',#2768,#786);
#578=LINE('',#2769,#787);
#579=LINE('',#2772,#788);
#580=LINE('',#2774,#789);
#581=LINE('',#2775,#790);
#582=LINE('',#2778,#791);
#583=LINE('',#2780,#792);
#584=LINE('',#2781,#793);
#585=LINE('',#2783,#794);
#586=LINE('',#2784,#795);
#587=LINE('',#2791,#796);
#588=LINE('',#2793,#797);
#589=LINE('',#2795,#798);
#590=LINE('',#2796,#799);
#591=LINE('',#2799,#800);
#592=LINE('',#2801,#801);
#593=LINE('',#2802,#802);
#594=LINE('',#2805,#803);
#595=LINE('',#2807,#804);
#596=LINE('',#2808,#805);
#597=LINE('',#2810,#806);
#598=LINE('',#2811,#807);
#599=LINE('',#2819,#808);
#600=VECTOR('',#1910,0.409999999999997);
#601=VECTOR('',#1919,0.409999999999997);
#602=VECTOR('',#1928,0.409999999999997);
#603=VECTOR('',#1937,0.409999999999997);
#604=VECTOR('',#1944,1.);
#605=VECTOR('',#1945,1.);
#606=VECTOR('',#1946,1.);
#607=VECTOR('',#1947,1.);
#608=VECTOR('',#1950,1.);
#609=VECTOR('',#1951,1.);
#610=VECTOR('',#1952,1.);
#611=VECTOR('',#1953,1.);
#612=VECTOR('',#1956,1.);
#613=VECTOR('',#1957,1.);
#614=VECTOR('',#1958,1.);
#615=VECTOR('',#1959,1.);
#616=VECTOR('',#1962,1.);
#617=VECTOR('',#1963,1.);
#618=VECTOR('',#1964,1.);
#619=VECTOR('',#1965,1.);
#620=VECTOR('',#1968,1.);
#621=VECTOR('',#1969,1.);
#622=VECTOR('',#1970,1.);
#623=VECTOR('',#1971,1.);
#624=VECTOR('',#1974,1.);
#625=VECTOR('',#1975,1.);
#626=VECTOR('',#1976,1.);
#627=VECTOR('',#1977,1.);
#628=VECTOR('',#1980,1.);
#629=VECTOR('',#1981,1.);
#630=VECTOR('',#1982,1.);
#631=VECTOR('',#1983,1.);
#632=VECTOR('',#1986,1.);
#633=VECTOR('',#1987,1.);
#634=VECTOR('',#1988,1.);
#635=VECTOR('',#1989,1.);
#636=VECTOR('',#1992,1.);
#637=VECTOR('',#1993,1.);
#638=VECTOR('',#1994,1.);
#639=VECTOR('',#1995,1.);
#640=VECTOR('',#1998,1.);
#641=VECTOR('',#1999,1.);
#642=VECTOR('',#2000,1.);
#643=VECTOR('',#2001,1.);
#644=VECTOR('',#2004,1.);
#645=VECTOR('',#2005,1.);
#646=VECTOR('',#2006,1.);
#647=VECTOR('',#2007,1.);
#648=VECTOR('',#2010,1.);
#649=VECTOR('',#2011,1.);
#650=VECTOR('',#2012,1.);
#651=VECTOR('',#2013,1.);
#652=VECTOR('',#2016,1.);
#653=VECTOR('',#2017,1.);
#654=VECTOR('',#2018,1.);
#655=VECTOR('',#2019,1.);
#656=VECTOR('',#2020,1.);
#657=VECTOR('',#2021,1.);
#658=VECTOR('',#2022,1.);
#659=VECTOR('',#2023,1.);
#660=VECTOR('',#2024,1.);
#661=VECTOR('',#2025,1.);
#662=VECTOR('',#2026,1.);
#663=VECTOR('',#2027,1.);
#664=VECTOR('',#2028,1.);
#665=VECTOR('',#2029,1.);
#666=VECTOR('',#2030,1.);
#667=VECTOR('',#2031,1.);
#668=VECTOR('',#2032,1.);
#669=VECTOR('',#2033,1.);
#670=VECTOR('',#2034,1.);
#671=VECTOR('',#2035,1.);
#672=VECTOR('',#2036,1.);
#673=VECTOR('',#2037,1.);
#674=VECTOR('',#2038,1.);
#675=VECTOR('',#2039,1.);
#676=VECTOR('',#2040,1.);
#677=VECTOR('',#2041,1.);
#678=VECTOR('',#2042,1.);
#679=VECTOR('',#2043,1.);
#680=VECTOR('',#2044,1.);
#681=VECTOR('',#2045,1.);
#682=VECTOR('',#2046,1.);
#683=VECTOR('',#2047,1.);
#684=VECTOR('',#2048,1.);
#685=VECTOR('',#2049,1.);
#686=VECTOR('',#2050,1.);
#687=VECTOR('',#2051,1.);
#688=VECTOR('',#2052,1.);
#689=VECTOR('',#2053,1.);
#690=VECTOR('',#2054,1.);
#691=VECTOR('',#2055,1.);
#692=VECTOR('',#2058,1.);
#693=VECTOR('',#2059,1.);
#694=VECTOR('',#2062,1.);
#695=VECTOR('',#2063,1.);
#696=VECTOR('',#2066,1.);
#697=VECTOR('',#2067,1.);
#698=VECTOR('',#2070,1.);
#699=VECTOR('',#2071,1.);
#700=VECTOR('',#2074,1.);
#701=VECTOR('',#2077,1.);
#702=VECTOR('',#2080,1.);
#703=VECTOR('',#2081,1.);
#704=VECTOR('',#2084,1.);
#705=VECTOR('',#2085,1.);
#706=VECTOR('',#2088,1.);
#707=VECTOR('',#2089,1.);
#708=VECTOR('',#2092,1.);
#709=VECTOR('',#2093,1.);
#710=VECTOR('',#2096,1.);
#711=VECTOR('',#2099,1.);
#712=VECTOR('',#2102,1.);
#713=VECTOR('',#2103,1.);
#714=VECTOR('',#2106,1.);
#715=VECTOR('',#2107,1.);
#716=VECTOR('',#2110,1.);
#717=VECTOR('',#2111,1.);
#718=VECTOR('',#2114,1.);
#719=VECTOR('',#2115,1.);
#720=VECTOR('',#2118,1.);
#721=VECTOR('',#2121,1.);
#722=VECTOR('',#2124,1.);
#723=VECTOR('',#2125,1.);
#724=VECTOR('',#2128,1.);
#725=VECTOR('',#2129,1.);
#726=VECTOR('',#2132,1.);
#727=VECTOR('',#2133,1.);
#728=VECTOR('',#2136,1.);
#729=VECTOR('',#2137,1.);
#730=VECTOR('',#2140,1.);
#731=VECTOR('',#2143,1.);
#732=VECTOR('',#2146,1.);
#733=VECTOR('',#2147,1.);
#734=VECTOR('',#2150,1.);
#735=VECTOR('',#2151,1.);
#736=VECTOR('',#2154,1.);
#737=VECTOR('',#2155,1.);
#738=VECTOR('',#2158,1.);
#739=VECTOR('',#2159,1.);
#740=VECTOR('',#2162,1.);
#741=VECTOR('',#2165,1.);
#742=VECTOR('',#2168,1.);
#743=VECTOR('',#2169,1.);
#744=VECTOR('',#2172,1.);
#745=VECTOR('',#2173,1.);
#746=VECTOR('',#2176,1.);
#747=VECTOR('',#2177,1.);
#748=VECTOR('',#2180,1.);
#749=VECTOR('',#2181,1.);
#750=VECTOR('',#2184,1.);
#751=VECTOR('',#2187,1.);
#752=VECTOR('',#2190,1.);
#753=VECTOR('',#2191,1.);
#754=VECTOR('',#2192,1.);
#755=VECTOR('',#2195,1.);
#756=VECTOR('',#2196,1.);
#757=VECTOR('',#2199,1.);
#758=VECTOR('',#2200,1.);
#759=VECTOR('',#2203,1.);
#760=VECTOR('',#2210,1.);
#761=VECTOR('',#2211,1.);
#762=VECTOR('',#2212,1.);
#763=VECTOR('',#2213,1.);
#764=VECTOR('',#2216,1.);
#765=VECTOR('',#2217,1.);
#766=VECTOR('',#2218,1.);
#767=VECTOR('',#2219,1.);
#768=VECTOR('',#2222,1.);
#769=VECTOR('',#2223,1.);
#770=VECTOR('',#2226,1.);
#771=VECTOR('',#2227,1.);
#772=VECTOR('',#2228,1.);
#773=VECTOR('',#2229,1.);
#774=VECTOR('',#2230,1.);
#775=VECTOR('',#2233,1.);
#776=VECTOR('',#2234,1.);
#777=VECTOR('',#2237,1.);
#778=VECTOR('',#2238,1.);
#779=VECTOR('',#2239,1.);
#780=VECTOR('',#2242,1.);
#781=VECTOR('',#2243,1.);
#782=VECTOR('',#2246,1.);
#783=VECTOR('',#2247,1.);
#784=VECTOR('',#2256,1.);
#785=VECTOR('',#2257,1.);
#786=VECTOR('',#2258,1.);
#787=VECTOR('',#2259,1.);
#788=VECTOR('',#2262,1.);
#789=VECTOR('',#2263,1.);
#790=VECTOR('',#2264,1.);
#791=VECTOR('',#2267,1.);
#792=VECTOR('',#2268,1.);
#793=VECTOR('',#2269,1.);
#794=VECTOR('',#2272,1.);
#795=VECTOR('',#2273,1.);
#796=VECTOR('',#2282,1.);
#797=VECTOR('',#2283,1.);
#798=VECTOR('',#2284,1.);
#799=VECTOR('',#2285,1.);
#800=VECTOR('',#2288,1.);
#801=VECTOR('',#2289,1.);
#802=VECTOR('',#2290,1.);
#803=VECTOR('',#2293,1.);
#804=VECTOR('',#2294,1.);
#805=VECTOR('',#2295,1.);
#806=VECTOR('',#2298,1.);
#807=VECTOR('',#2299,1.);
#808=VECTOR('',#2310,0.4);
#809=CIRCLE('',#1778,0.409999999999997);
#810=CIRCLE('',#1779,0.409999999999997);
#811=CIRCLE('',#1782,0.409999999999997);
#812=CIRCLE('',#1783,0.409999999999997);
#813=CIRCLE('',#1786,0.409999999999997);
#814=CIRCLE('',#1787,0.409999999999997);
#815=CIRCLE('',#1790,0.409999999999997);
#816=CIRCLE('',#1791,0.409999999999997);
#817=CIRCLE('',#1874,0.4);
#818=CIRCLE('',#1875,0.4);
#819=VERTEX_POINT('',#2368);
#820=VERTEX_POINT('',#2370);
#821=VERTEX_POINT('',#2375);
#822=VERTEX_POINT('',#2377);
#823=VERTEX_POINT('',#2382);
#824=VERTEX_POINT('',#2384);
#825=VERTEX_POINT('',#2389);
#826=VERTEX_POINT('',#2391);
#827=VERTEX_POINT('',#2396);
#828=VERTEX_POINT('',#2397);
#829=VERTEX_POINT('',#2399);
#830=VERTEX_POINT('',#2401);
#831=VERTEX_POINT('',#2405);
#832=VERTEX_POINT('',#2406);
#833=VERTEX_POINT('',#2408);
#834=VERTEX_POINT('',#2410);
#835=VERTEX_POINT('',#2414);
#836=VERTEX_POINT('',#2415);
#837=VERTEX_POINT('',#2417);
#838=VERTEX_POINT('',#2419);
#839=VERTEX_POINT('',#2423);
#840=VERTEX_POINT('',#2424);
#841=VERTEX_POINT('',#2426);
#842=VERTEX_POINT('',#2428);
#843=VERTEX_POINT('',#2432);
#844=VERTEX_POINT('',#2433);
#845=VERTEX_POINT('',#2435);
#846=VERTEX_POINT('',#2437);
#847=VERTEX_POINT('',#2441);
#848=VERTEX_POINT('',#2442);
#849=VERTEX_POINT('',#2444);
#850=VERTEX_POINT('',#2446);
#851=VERTEX_POINT('',#2450);
#852=VERTEX_POINT('',#2451);
#853=VERTEX_POINT('',#2453);
#854=VERTEX_POINT('',#2455);
#855=VERTEX_POINT('',#2459);
#856=VERTEX_POINT('',#2460);
#857=VERTEX_POINT('',#2462);
#858=VERTEX_POINT('',#2464);
#859=VERTEX_POINT('',#2468);
#860=VERTEX_POINT('',#2469);
#861=VERTEX_POINT('',#2471);
#862=VERTEX_POINT('',#2473);
#863=VERTEX_POINT('',#2477);
#864=VERTEX_POINT('',#2478);
#865=VERTEX_POINT('',#2480);
#866=VERTEX_POINT('',#2482);
#867=VERTEX_POINT('',#2486);
#868=VERTEX_POINT('',#2487);
#869=VERTEX_POINT('',#2489);
#870=VERTEX_POINT('',#2491);
#871=VERTEX_POINT('',#2495);
#872=VERTEX_POINT('',#2496);
#873=VERTEX_POINT('',#2498);
#874=VERTEX_POINT('',#2500);
#875=VERTEX_POINT('',#2504);
#876=VERTEX_POINT('',#2506);
#877=VERTEX_POINT('',#2508);
#878=VERTEX_POINT('',#2510);
#879=VERTEX_POINT('',#2513);
#880=VERTEX_POINT('',#2515);
#881=VERTEX_POINT('',#2518);
#882=VERTEX_POINT('',#2520);
#883=VERTEX_POINT('',#2523);
#884=VERTEX_POINT('',#2525);
#885=VERTEX_POINT('',#2528);
#886=VERTEX_POINT('',#2530);
#887=VERTEX_POINT('',#2533);
#888=VERTEX_POINT('',#2535);
#889=VERTEX_POINT('',#2538);
#890=VERTEX_POINT('',#2540);
#891=VERTEX_POINT('',#2542);
#892=VERTEX_POINT('',#2544);
#893=VERTEX_POINT('',#2547);
#894=VERTEX_POINT('',#2549);
#895=VERTEX_POINT('',#2552);
#896=VERTEX_POINT('',#2554);
#897=VERTEX_POINT('',#2557);
#898=VERTEX_POINT('',#2559);
#899=VERTEX_POINT('',#2562);
#900=VERTEX_POINT('',#2564);
#901=VERTEX_POINT('',#2567);
#902=VERTEX_POINT('',#2569);
#903=VERTEX_POINT('',#2573);
#904=VERTEX_POINT('',#2577);
#905=VERTEX_POINT('',#2581);
#906=VERTEX_POINT('',#2585);
#907=VERTEX_POINT('',#2593);
#908=VERTEX_POINT('',#2597);
#909=VERTEX_POINT('',#2601);
#910=VERTEX_POINT('',#2605);
#911=VERTEX_POINT('',#2613);
#912=VERTEX_POINT('',#2617);
#913=VERTEX_POINT('',#2621);
#914=VERTEX_POINT('',#2625);
#915=VERTEX_POINT('',#2633);
#916=VERTEX_POINT('',#2637);
#917=VERTEX_POINT('',#2641);
#918=VERTEX_POINT('',#2645);
#919=VERTEX_POINT('',#2653);
#920=VERTEX_POINT('',#2657);
#921=VERTEX_POINT('',#2661);
#922=VERTEX_POINT('',#2665);
#923=VERTEX_POINT('',#2673);
#924=VERTEX_POINT('',#2677);
#925=VERTEX_POINT('',#2681);
#926=VERTEX_POINT('',#2685);
#927=VERTEX_POINT('',#2693);
#928=VERTEX_POINT('',#2695);
#929=VERTEX_POINT('',#2699);
#930=VERTEX_POINT('',#2703);
#931=VERTEX_POINT('',#2711);
#932=VERTEX_POINT('',#2712);
#933=VERTEX_POINT('',#2714);
#934=VERTEX_POINT('',#2716);
#935=VERTEX_POINT('',#2720);
#936=VERTEX_POINT('',#2721);
#937=VERTEX_POINT('',#2723);
#938=VERTEX_POINT('',#2725);
#939=VERTEX_POINT('',#2732);
#940=VERTEX_POINT('',#2734);
#941=VERTEX_POINT('',#2736);
#942=VERTEX_POINT('',#2738);
#943=VERTEX_POINT('',#2742);
#944=VERTEX_POINT('',#2746);
#945=VERTEX_POINT('',#2748);
#946=VERTEX_POINT('',#2752);
#947=VERTEX_POINT('',#2762);
#948=VERTEX_POINT('',#2763);
#949=VERTEX_POINT('',#2765);
#950=VERTEX_POINT('',#2767);
#951=VERTEX_POINT('',#2771);
#952=VERTEX_POINT('',#2773);
#953=VERTEX_POINT('',#2777);
#954=VERTEX_POINT('',#2779);
#955=VERTEX_POINT('',#2789);
#956=VERTEX_POINT('',#2790);
#957=VERTEX_POINT('',#2792);
#958=VERTEX_POINT('',#2794);
#959=VERTEX_POINT('',#2798);
#960=VERTEX_POINT('',#2800);
#961=VERTEX_POINT('',#2804);
#962=VERTEX_POINT('',#2806);
#963=VERTEX_POINT('',#2816);
#964=VERTEX_POINT('',#2818);
#965=EDGE_CURVE('',#819,#819,#809,.T.);
#966=EDGE_CURVE('',#819,#820,#391,.T.);
#967=EDGE_CURVE('',#820,#820,#810,.T.);
#968=EDGE_CURVE('',#821,#821,#811,.T.);
#969=EDGE_CURVE('',#821,#822,#392,.T.);
#970=EDGE_CURVE('',#822,#822,#812,.T.);
#971=EDGE_CURVE('',#823,#823,#813,.T.);
#972=EDGE_CURVE('',#823,#824,#393,.T.);
#973=EDGE_CURVE('',#824,#824,#814,.T.);
#974=EDGE_CURVE('',#825,#825,#815,.T.);
#975=EDGE_CURVE('',#825,#826,#394,.T.);
#976=EDGE_CURVE('',#826,#826,#816,.T.);
#977=EDGE_CURVE('',#827,#828,#395,.T.);
#978=EDGE_CURVE('',#829,#827,#396,.T.);
#979=EDGE_CURVE('',#830,#829,#397,.T.);
#980=EDGE_CURVE('',#828,#830,#398,.T.);
#981=EDGE_CURVE('',#831,#832,#399,.T.);
#982=EDGE_CURVE('',#833,#831,#400,.T.);
#983=EDGE_CURVE('',#834,#833,#401,.T.);
#984=EDGE_CURVE('',#832,#834,#402,.T.);
#985=EDGE_CURVE('',#835,#836,#403,.T.);
#986=EDGE_CURVE('',#837,#835,#404,.T.);
#987=EDGE_CURVE('',#838,#837,#405,.T.);
#988=EDGE_CURVE('',#836,#838,#406,.T.);
#989=EDGE_CURVE('',#839,#840,#407,.T.);
#990=EDGE_CURVE('',#841,#839,#408,.T.);
#991=EDGE_CURVE('',#842,#841,#409,.T.);
#992=EDGE_CURVE('',#840,#842,#410,.T.);
#993=EDGE_CURVE('',#843,#844,#411,.T.);
#994=EDGE_CURVE('',#845,#843,#412,.T.);
#995=EDGE_CURVE('',#846,#845,#413,.T.);
#996=EDGE_CURVE('',#844,#846,#414,.T.);
#997=EDGE_CURVE('',#847,#848,#415,.T.);
#998=EDGE_CURVE('',#849,#847,#416,.T.);
#999=EDGE_CURVE('',#850,#849,#417,.T.);
#1000=EDGE_CURVE('',#848,#850,#418,.T.);
#1001=EDGE_CURVE('',#851,#852,#419,.T.);
#1002=EDGE_CURVE('',#853,#851,#420,.T.);
#1003=EDGE_CURVE('',#854,#853,#421,.T.);
#1004=EDGE_CURVE('',#854,#852,#422,.T.);
#1005=EDGE_CURVE('',#855,#856,#423,.T.);
#1006=EDGE_CURVE('',#857,#855,#424,.T.);
#1007=EDGE_CURVE('',#858,#857,#425,.T.);
#1008=EDGE_CURVE('',#858,#856,#426,.T.);
#1009=EDGE_CURVE('',#859,#860,#427,.T.);
#1010=EDGE_CURVE('',#861,#859,#428,.T.);
#1011=EDGE_CURVE('',#862,#861,#429,.T.);
#1012=EDGE_CURVE('',#862,#860,#430,.T.);
#1013=EDGE_CURVE('',#863,#864,#431,.T.);
#1014=EDGE_CURVE('',#865,#863,#432,.T.);
#1015=EDGE_CURVE('',#866,#865,#433,.T.);
#1016=EDGE_CURVE('',#866,#864,#434,.T.);
#1017=EDGE_CURVE('',#867,#868,#435,.T.);
#1018=EDGE_CURVE('',#869,#867,#436,.T.);
#1019=EDGE_CURVE('',#870,#869,#437,.T.);
#1020=EDGE_CURVE('',#870,#868,#438,.T.);
#1021=EDGE_CURVE('',#871,#872,#439,.T.);
#1022=EDGE_CURVE('',#873,#871,#440,.T.);
#1023=EDGE_CURVE('',#874,#873,#441,.T.);
#1024=EDGE_CURVE('',#874,#872,#442,.T.);
#1025=EDGE_CURVE('',#875,#847,#443,.T.);
#1026=EDGE_CURVE('',#876,#875,#444,.T.);
#1027=EDGE_CURVE('',#877,#876,#445,.T.);
#1028=EDGE_CURVE('',#878,#877,#446,.T.);
#1029=EDGE_CURVE('',#872,#878,#447,.T.);
#1030=EDGE_CURVE('',#874,#879,#448,.T.);
#1031=EDGE_CURVE('',#880,#879,#449,.T.);
#1032=EDGE_CURVE('',#868,#880,#450,.T.);
#1033=EDGE_CURVE('',#870,#881,#451,.T.);
#1034=EDGE_CURVE('',#882,#881,#452,.T.);
#1035=EDGE_CURVE('',#864,#882,#453,.T.);
#1036=EDGE_CURVE('',#866,#883,#454,.T.);
#1037=EDGE_CURVE('',#884,#883,#455,.T.);
#1038=EDGE_CURVE('',#860,#884,#456,.T.);
#1039=EDGE_CURVE('',#862,#885,#457,.T.);
#1040=EDGE_CURVE('',#886,#885,#458,.T.);
#1041=EDGE_CURVE('',#856,#886,#459,.T.);
#1042=EDGE_CURVE('',#858,#887,#460,.T.);
#1043=EDGE_CURVE('',#888,#887,#461,.T.);
#1044=EDGE_CURVE('',#852,#888,#462,.T.);
#1045=EDGE_CURVE('',#854,#889,#463,.T.);
#1046=EDGE_CURVE('',#890,#889,#464,.T.);
#1047=EDGE_CURVE('',#891,#890,#465,.T.);
#1048=EDGE_CURVE('',#892,#891,#466,.T.);
#1049=EDGE_CURVE('',#892,#845,#467,.T.);
#1050=EDGE_CURVE('',#893,#843,#468,.T.);
#1051=EDGE_CURVE('',#894,#893,#469,.T.);
#1052=EDGE_CURVE('',#894,#841,#470,.T.);
#1053=EDGE_CURVE('',#895,#839,#471,.T.);
#1054=EDGE_CURVE('',#896,#895,#472,.T.);
#1055=EDGE_CURVE('',#896,#837,#473,.T.);
#1056=EDGE_CURVE('',#897,#835,#474,.T.);
#1057=EDGE_CURVE('',#898,#897,#475,.T.);
#1058=EDGE_CURVE('',#898,#833,#476,.T.);
#1059=EDGE_CURVE('',#899,#831,#477,.T.);
#1060=EDGE_CURVE('',#900,#899,#478,.T.);
#1061=EDGE_CURVE('',#900,#829,#479,.T.);
#1062=EDGE_CURVE('',#901,#827,#480,.T.);
#1063=EDGE_CURVE('',#902,#901,#481,.T.);
#1064=EDGE_CURVE('',#902,#849,#482,.T.);
#1065=EDGE_CURVE('',#903,#878,#483,.T.);
#1066=EDGE_CURVE('',#871,#903,#484,.T.);
#1067=EDGE_CURVE('',#904,#848,#485,.T.);
#1068=EDGE_CURVE('',#875,#904,#486,.T.);
#1069=EDGE_CURVE('',#905,#903,#487,.T.);
#1070=EDGE_CURVE('',#905,#873,#488,.T.);
#1071=EDGE_CURVE('',#850,#906,#489,.T.);
#1072=EDGE_CURVE('',#906,#904,#490,.T.);
#1073=EDGE_CURVE('',#879,#905,#491,.T.);
#1074=EDGE_CURVE('',#906,#902,#492,.T.);
#1075=EDGE_CURVE('',#907,#880,#493,.T.);
#1076=EDGE_CURVE('',#867,#907,#494,.T.);
#1077=EDGE_CURVE('',#908,#828,#495,.T.);
#1078=EDGE_CURVE('',#901,#908,#496,.T.);
#1079=EDGE_CURVE('',#909,#907,#497,.T.);
#1080=EDGE_CURVE('',#909,#869,#498,.T.);
#1081=EDGE_CURVE('',#830,#910,#499,.T.);
#1082=EDGE_CURVE('',#910,#908,#500,.T.);
#1083=EDGE_CURVE('',#881,#909,#501,.T.);
#1084=EDGE_CURVE('',#910,#900,#502,.T.);
#1085=EDGE_CURVE('',#911,#882,#503,.T.);
#1086=EDGE_CURVE('',#863,#911,#504,.T.);
#1087=EDGE_CURVE('',#912,#832,#505,.T.);
#1088=EDGE_CURVE('',#899,#912,#506,.T.);
#1089=EDGE_CURVE('',#913,#911,#507,.T.);
#1090=EDGE_CURVE('',#913,#865,#508,.T.);
#1091=EDGE_CURVE('',#834,#914,#509,.T.);
#1092=EDGE_CURVE('',#914,#912,#510,.T.);
#1093=EDGE_CURVE('',#883,#913,#511,.T.);
#1094=EDGE_CURVE('',#914,#898,#512,.T.);
#1095=EDGE_CURVE('',#915,#884,#513,.T.);
#1096=EDGE_CURVE('',#859,#915,#514,.T.);
#1097=EDGE_CURVE('',#916,#836,#515,.T.);
#1098=EDGE_CURVE('',#897,#916,#516,.T.);
#1099=EDGE_CURVE('',#917,#915,#517,.T.);
#1100=EDGE_CURVE('',#917,#861,#518,.T.);
#1101=EDGE_CURVE('',#838,#918,#519,.T.);
#1102=EDGE_CURVE('',#918,#916,#520,.T.);
#1103=EDGE_CURVE('',#885,#917,#521,.T.);
#1104=EDGE_CURVE('',#918,#896,#522,.T.);
#1105=EDGE_CURVE('',#919,#886,#523,.T.);
#1106=EDGE_CURVE('',#855,#919,#524,.T.);
#1107=EDGE_CURVE('',#920,#840,#525,.T.);
#1108=EDGE_CURVE('',#895,#920,#526,.T.);
#1109=EDGE_CURVE('',#921,#919,#527,.T.);
#1110=EDGE_CURVE('',#921,#857,#528,.T.);
#1111=EDGE_CURVE('',#842,#922,#529,.T.);
#1112=EDGE_CURVE('',#922,#920,#530,.T.);
#1113=EDGE_CURVE('',#887,#921,#531,.T.);
#1114=EDGE_CURVE('',#922,#894,#532,.T.);
#1115=EDGE_CURVE('',#923,#888,#533,.T.);
#1116=EDGE_CURVE('',#851,#923,#534,.T.);
#1117=EDGE_CURVE('',#924,#844,#535,.T.);
#1118=EDGE_CURVE('',#893,#924,#536,.T.);
#1119=EDGE_CURVE('',#925,#923,#537,.T.);
#1120=EDGE_CURVE('',#925,#853,#538,.T.);
#1121=EDGE_CURVE('',#846,#926,#539,.T.);
#1122=EDGE_CURVE('',#926,#924,#540,.T.);
#1123=EDGE_CURVE('',#889,#925,#541,.T.);
#1124=EDGE_CURVE('',#926,#892,#542,.T.);
#1125=EDGE_CURVE('',#891,#927,#543,.T.);
#1126=EDGE_CURVE('',#927,#928,#544,.T.);
#1127=EDGE_CURVE('',#876,#928,#545,.T.);
#1128=EDGE_CURVE('',#929,#890,#546,.T.);
#1129=EDGE_CURVE('',#927,#929,#547,.T.);
#1130=EDGE_CURVE('',#930,#877,#548,.T.);
#1131=EDGE_CURVE('',#929,#930,#549,.T.);
#1132=EDGE_CURVE('',#928,#930,#550,.T.);
#1133=EDGE_CURVE('',#931,#932,#551,.T.);
#1134=EDGE_CURVE('',#933,#931,#552,.T.);
#1135=EDGE_CURVE('',#934,#933,#553,.T.);
#1136=EDGE_CURVE('',#932,#934,#554,.T.);
#1137=EDGE_CURVE('',#935,#936,#555,.T.);
#1138=EDGE_CURVE('',#937,#935,#556,.T.);
#1139=EDGE_CURVE('',#938,#937,#557,.T.);
#1140=EDGE_CURVE('',#936,#938,#558,.T.);
#1141=EDGE_CURVE('',#934,#937,#559,.T.);
#1142=EDGE_CURVE('',#938,#933,#560,.T.);
#1143=EDGE_CURVE('',#939,#931,#561,.T.);
#1144=EDGE_CURVE('',#940,#939,#562,.T.);
#1145=EDGE_CURVE('',#940,#941,#563,.T.);
#1146=EDGE_CURVE('',#941,#942,#564,.T.);
#1147=EDGE_CURVE('',#936,#942,#565,.T.);
#1148=EDGE_CURVE('',#932,#943,#566,.T.);
#1149=EDGE_CURVE('',#943,#939,#567,.T.);
#1150=EDGE_CURVE('',#941,#944,#568,.T.);
#1151=EDGE_CURVE('',#944,#945,#569,.T.);
#1152=EDGE_CURVE('',#942,#945,#570,.T.);
#1153=EDGE_CURVE('',#946,#940,#571,.T.);
#1154=EDGE_CURVE('',#946,#943,#572,.T.);
#1155=EDGE_CURVE('',#945,#935,#573,.T.);
#1156=EDGE_CURVE('',#944,#946,#574,.T.);
#1157=EDGE_CURVE('',#947,#948,#575,.T.);
#1158=EDGE_CURVE('',#948,#949,#576,.T.);
#1159=EDGE_CURVE('',#950,#949,#577,.T.);
#1160=EDGE_CURVE('',#947,#950,#578,.T.);
#1161=EDGE_CURVE('',#951,#947,#579,.T.);
#1162=EDGE_CURVE('',#952,#950,#580,.T.);
#1163=EDGE_CURVE('',#951,#952,#581,.T.);
#1164=EDGE_CURVE('',#953,#951,#582,.T.);
#1165=EDGE_CURVE('',#954,#952,#583,.T.);
#1166=EDGE_CURVE('',#953,#954,#584,.T.);
#1167=EDGE_CURVE('',#948,#953,#585,.T.);
#1168=EDGE_CURVE('',#949,#954,#586,.T.);
#1169=EDGE_CURVE('',#955,#956,#587,.T.);
#1170=EDGE_CURVE('',#956,#957,#588,.T.);
#1171=EDGE_CURVE('',#958,#957,#589,.T.);
#1172=EDGE_CURVE('',#955,#958,#590,.T.);
#1173=EDGE_CURVE('',#959,#955,#591,.T.);
#1174=EDGE_CURVE('',#960,#958,#592,.T.);
#1175=EDGE_CURVE('',#959,#960,#593,.T.);
#1176=EDGE_CURVE('',#961,#959,#594,.T.);
#1177=EDGE_CURVE('',#962,#960,#595,.T.);
#1178=EDGE_CURVE('',#961,#962,#596,.T.);
#1179=EDGE_CURVE('',#956,#961,#597,.T.);
#1180=EDGE_CURVE('',#957,#962,#598,.T.);
#1181=EDGE_CURVE('',#963,#963,#817,.T.);
#1182=EDGE_CURVE('',#963,#964,#599,.T.);
#1183=EDGE_CURVE('',#964,#964,#818,.T.);
#1184=ORIENTED_EDGE('',*,*,#965,.F.);
#1185=ORIENTED_EDGE('',*,*,#966,.T.);
#1186=ORIENTED_EDGE('',*,*,#967,.T.);
#1187=ORIENTED_EDGE('',*,*,#966,.F.);
#1188=ORIENTED_EDGE('',*,*,#967,.F.);
#1189=ORIENTED_EDGE('',*,*,#968,.F.);
#1190=ORIENTED_EDGE('',*,*,#969,.T.);
#1191=ORIENTED_EDGE('',*,*,#970,.T.);
#1192=ORIENTED_EDGE('',*,*,#969,.F.);
#1193=ORIENTED_EDGE('',*,*,#970,.F.);
#1194=ORIENTED_EDGE('',*,*,#971,.F.);
#1195=ORIENTED_EDGE('',*,*,#972,.T.);
#1196=ORIENTED_EDGE('',*,*,#973,.T.);
#1197=ORIENTED_EDGE('',*,*,#972,.F.);
#1198=ORIENTED_EDGE('',*,*,#973,.F.);
#1199=ORIENTED_EDGE('',*,*,#974,.F.);
#1200=ORIENTED_EDGE('',*,*,#975,.T.);
#1201=ORIENTED_EDGE('',*,*,#976,.T.);
#1202=ORIENTED_EDGE('',*,*,#975,.F.);
#1203=ORIENTED_EDGE('',*,*,#976,.F.);
#1204=ORIENTED_EDGE('',*,*,#977,.F.);
#1205=ORIENTED_EDGE('',*,*,#978,.F.);
#1206=ORIENTED_EDGE('',*,*,#979,.F.);
#1207=ORIENTED_EDGE('',*,*,#980,.F.);
#1208=ORIENTED_EDGE('',*,*,#981,.F.);
#1209=ORIENTED_EDGE('',*,*,#982,.F.);
#1210=ORIENTED_EDGE('',*,*,#983,.F.);
#1211=ORIENTED_EDGE('',*,*,#984,.F.);
#1212=ORIENTED_EDGE('',*,*,#985,.F.);
#1213=ORIENTED_EDGE('',*,*,#986,.F.);
#1214=ORIENTED_EDGE('',*,*,#987,.F.);
#1215=ORIENTED_EDGE('',*,*,#988,.F.);
#1216=ORIENTED_EDGE('',*,*,#989,.F.);
#1217=ORIENTED_EDGE('',*,*,#990,.F.);
#1218=ORIENTED_EDGE('',*,*,#991,.F.);
#1219=ORIENTED_EDGE('',*,*,#992,.F.);
#1220=ORIENTED_EDGE('',*,*,#993,.F.);
#1221=ORIENTED_EDGE('',*,*,#994,.F.);
#1222=ORIENTED_EDGE('',*,*,#995,.F.);
#1223=ORIENTED_EDGE('',*,*,#996,.F.);
#1224=ORIENTED_EDGE('',*,*,#997,.F.);
#1225=ORIENTED_EDGE('',*,*,#998,.F.);
#1226=ORIENTED_EDGE('',*,*,#999,.F.);
#1227=ORIENTED_EDGE('',*,*,#1000,.F.);
#1228=ORIENTED_EDGE('',*,*,#1001,.F.);
#1229=ORIENTED_EDGE('',*,*,#1002,.F.);
#1230=ORIENTED_EDGE('',*,*,#1003,.F.);
#1231=ORIENTED_EDGE('',*,*,#1004,.T.);
#1232=ORIENTED_EDGE('',*,*,#1005,.F.);
#1233=ORIENTED_EDGE('',*,*,#1006,.F.);
#1234=ORIENTED_EDGE('',*,*,#1007,.F.);
#1235=ORIENTED_EDGE('',*,*,#1008,.T.);
#1236=ORIENTED_EDGE('',*,*,#1009,.F.);
#1237=ORIENTED_EDGE('',*,*,#1010,.F.);
#1238=ORIENTED_EDGE('',*,*,#1011,.F.);
#1239=ORIENTED_EDGE('',*,*,#1012,.T.);
#1240=ORIENTED_EDGE('',*,*,#1013,.F.);
#1241=ORIENTED_EDGE('',*,*,#1014,.F.);
#1242=ORIENTED_EDGE('',*,*,#1015,.F.);
#1243=ORIENTED_EDGE('',*,*,#1016,.T.);
#1244=ORIENTED_EDGE('',*,*,#1017,.F.);
#1245=ORIENTED_EDGE('',*,*,#1018,.F.);
#1246=ORIENTED_EDGE('',*,*,#1019,.F.);
#1247=ORIENTED_EDGE('',*,*,#1020,.T.);
#1248=ORIENTED_EDGE('',*,*,#1021,.F.);
#1249=ORIENTED_EDGE('',*,*,#1022,.F.);
#1250=ORIENTED_EDGE('',*,*,#1023,.F.);
#1251=ORIENTED_EDGE('',*,*,#1024,.T.);
#1252=ORIENTED_EDGE('',*,*,#1025,.F.);
#1253=ORIENTED_EDGE('',*,*,#1026,.F.);
#1254=ORIENTED_EDGE('',*,*,#1027,.F.);
#1255=ORIENTED_EDGE('',*,*,#1028,.F.);
#1256=ORIENTED_EDGE('',*,*,#1029,.F.);
#1257=ORIENTED_EDGE('',*,*,#1024,.F.);
#1258=ORIENTED_EDGE('',*,*,#1030,.T.);
#1259=ORIENTED_EDGE('',*,*,#1031,.F.);
#1260=ORIENTED_EDGE('',*,*,#1032,.F.);
#1261=ORIENTED_EDGE('',*,*,#1020,.F.);
#1262=ORIENTED_EDGE('',*,*,#1033,.T.);
#1263=ORIENTED_EDGE('',*,*,#1034,.F.);
#1264=ORIENTED_EDGE('',*,*,#1035,.F.);
#1265=ORIENTED_EDGE('',*,*,#1016,.F.);
#1266=ORIENTED_EDGE('',*,*,#1036,.T.);
#1267=ORIENTED_EDGE('',*,*,#1037,.F.);
#1268=ORIENTED_EDGE('',*,*,#1038,.F.);
#1269=ORIENTED_EDGE('',*,*,#1012,.F.);
#1270=ORIENTED_EDGE('',*,*,#1039,.T.);
#1271=ORIENTED_EDGE('',*,*,#1040,.F.);
#1272=ORIENTED_EDGE('',*,*,#1041,.F.);
#1273=ORIENTED_EDGE('',*,*,#1008,.F.);
#1274=ORIENTED_EDGE('',*,*,#1042,.T.);
#1275=ORIENTED_EDGE('',*,*,#1043,.F.);
#1276=ORIENTED_EDGE('',*,*,#1044,.F.);
#1277=ORIENTED_EDGE('',*,*,#1004,.F.);
#1278=ORIENTED_EDGE('',*,*,#1045,.T.);
#1279=ORIENTED_EDGE('',*,*,#1046,.F.);
#1280=ORIENTED_EDGE('',*,*,#1047,.F.);
#1281=ORIENTED_EDGE('',*,*,#1048,.F.);
#1282=ORIENTED_EDGE('',*,*,#1049,.T.);
#1283=ORIENTED_EDGE('',*,*,#994,.T.);
#1284=ORIENTED_EDGE('',*,*,#1050,.F.);
#1285=ORIENTED_EDGE('',*,*,#1051,.F.);
#1286=ORIENTED_EDGE('',*,*,#1052,.T.);
#1287=ORIENTED_EDGE('',*,*,#990,.T.);
#1288=ORIENTED_EDGE('',*,*,#1053,.F.);
#1289=ORIENTED_EDGE('',*,*,#1054,.F.);
#1290=ORIENTED_EDGE('',*,*,#1055,.T.);
#1291=ORIENTED_EDGE('',*,*,#986,.T.);
#1292=ORIENTED_EDGE('',*,*,#1056,.F.);
#1293=ORIENTED_EDGE('',*,*,#1057,.F.);
#1294=ORIENTED_EDGE('',*,*,#1058,.T.);
#1295=ORIENTED_EDGE('',*,*,#982,.T.);
#1296=ORIENTED_EDGE('',*,*,#1059,.F.);
#1297=ORIENTED_EDGE('',*,*,#1060,.F.);
#1298=ORIENTED_EDGE('',*,*,#1061,.T.);
#1299=ORIENTED_EDGE('',*,*,#978,.T.);
#1300=ORIENTED_EDGE('',*,*,#1062,.F.);
#1301=ORIENTED_EDGE('',*,*,#1063,.F.);
#1302=ORIENTED_EDGE('',*,*,#1064,.T.);
#1303=ORIENTED_EDGE('',*,*,#998,.T.);
#1304=ORIENTED_EDGE('',*,*,#1021,.T.);
#1305=ORIENTED_EDGE('',*,*,#1029,.T.);
#1306=ORIENTED_EDGE('',*,*,#1065,.F.);
#1307=ORIENTED_EDGE('',*,*,#1066,.F.);
#1308=ORIENTED_EDGE('',*,*,#997,.T.);
#1309=ORIENTED_EDGE('',*,*,#1067,.F.);
#1310=ORIENTED_EDGE('',*,*,#1068,.F.);
#1311=ORIENTED_EDGE('',*,*,#1025,.T.);
#1312=ORIENTED_EDGE('',*,*,#1022,.T.);
#1313=ORIENTED_EDGE('',*,*,#1066,.T.);
#1314=ORIENTED_EDGE('',*,*,#1069,.F.);
#1315=ORIENTED_EDGE('',*,*,#1070,.T.);
#1316=ORIENTED_EDGE('',*,*,#1000,.T.);
#1317=ORIENTED_EDGE('',*,*,#1071,.T.);
#1318=ORIENTED_EDGE('',*,*,#1072,.T.);
#1319=ORIENTED_EDGE('',*,*,#1067,.T.);
#1320=ORIENTED_EDGE('',*,*,#1023,.T.);
#1321=ORIENTED_EDGE('',*,*,#1070,.F.);
#1322=ORIENTED_EDGE('',*,*,#1073,.F.);
#1323=ORIENTED_EDGE('',*,*,#1030,.F.);
#1324=ORIENTED_EDGE('',*,*,#999,.T.);
#1325=ORIENTED_EDGE('',*,*,#1064,.F.);
#1326=ORIENTED_EDGE('',*,*,#1074,.F.);
#1327=ORIENTED_EDGE('',*,*,#1071,.F.);
#1328=ORIENTED_EDGE('',*,*,#1017,.T.);
#1329=ORIENTED_EDGE('',*,*,#1032,.T.);
#1330=ORIENTED_EDGE('',*,*,#1075,.F.);
#1331=ORIENTED_EDGE('',*,*,#1076,.F.);
#1332=ORIENTED_EDGE('',*,*,#977,.T.);
#1333=ORIENTED_EDGE('',*,*,#1077,.F.);
#1334=ORIENTED_EDGE('',*,*,#1078,.F.);
#1335=ORIENTED_EDGE('',*,*,#1062,.T.);
#1336=ORIENTED_EDGE('',*,*,#1018,.T.);
#1337=ORIENTED_EDGE('',*,*,#1076,.T.);
#1338=ORIENTED_EDGE('',*,*,#1079,.F.);
#1339=ORIENTED_EDGE('',*,*,#1080,.T.);
#1340=ORIENTED_EDGE('',*,*,#980,.T.);
#1341=ORIENTED_EDGE('',*,*,#1081,.T.);
#1342=ORIENTED_EDGE('',*,*,#1082,.T.);
#1343=ORIENTED_EDGE('',*,*,#1077,.T.);
#1344=ORIENTED_EDGE('',*,*,#1019,.T.);
#1345=ORIENTED_EDGE('',*,*,#1080,.F.);
#1346=ORIENTED_EDGE('',*,*,#1083,.F.);
#1347=ORIENTED_EDGE('',*,*,#1033,.F.);
#1348=ORIENTED_EDGE('',*,*,#979,.T.);
#1349=ORIENTED_EDGE('',*,*,#1061,.F.);
#1350=ORIENTED_EDGE('',*,*,#1084,.F.);
#1351=ORIENTED_EDGE('',*,*,#1081,.F.);
#1352=ORIENTED_EDGE('',*,*,#1013,.T.);
#1353=ORIENTED_EDGE('',*,*,#1035,.T.);
#1354=ORIENTED_EDGE('',*,*,#1085,.F.);
#1355=ORIENTED_EDGE('',*,*,#1086,.F.);
#1356=ORIENTED_EDGE('',*,*,#981,.T.);
#1357=ORIENTED_EDGE('',*,*,#1087,.F.);
#1358=ORIENTED_EDGE('',*,*,#1088,.F.);
#1359=ORIENTED_EDGE('',*,*,#1059,.T.);
#1360=ORIENTED_EDGE('',*,*,#1014,.T.);
#1361=ORIENTED_EDGE('',*,*,#1086,.T.);
#1362=ORIENTED_EDGE('',*,*,#1089,.F.);
#1363=ORIENTED_EDGE('',*,*,#1090,.T.);
#1364=ORIENTED_EDGE('',*,*,#984,.T.);
#1365=ORIENTED_EDGE('',*,*,#1091,.T.);
#1366=ORIENTED_EDGE('',*,*,#1092,.T.);
#1367=ORIENTED_EDGE('',*,*,#1087,.T.);
#1368=ORIENTED_EDGE('',*,*,#1015,.T.);
#1369=ORIENTED_EDGE('',*,*,#1090,.F.);
#1370=ORIENTED_EDGE('',*,*,#1093,.F.);
#1371=ORIENTED_EDGE('',*,*,#1036,.F.);
#1372=ORIENTED_EDGE('',*,*,#983,.T.);
#1373=ORIENTED_EDGE('',*,*,#1058,.F.);
#1374=ORIENTED_EDGE('',*,*,#1094,.F.);
#1375=ORIENTED_EDGE('',*,*,#1091,.F.);
#1376=ORIENTED_EDGE('',*,*,#1009,.T.);
#1377=ORIENTED_EDGE('',*,*,#1038,.T.);
#1378=ORIENTED_EDGE('',*,*,#1095,.F.);
#1379=ORIENTED_EDGE('',*,*,#1096,.F.);
#1380=ORIENTED_EDGE('',*,*,#985,.T.);
#1381=ORIENTED_EDGE('',*,*,#1097,.F.);
#1382=ORIENTED_EDGE('',*,*,#1098,.F.);
#1383=ORIENTED_EDGE('',*,*,#1056,.T.);
#1384=ORIENTED_EDGE('',*,*,#1010,.T.);
#1385=ORIENTED_EDGE('',*,*,#1096,.T.);
#1386=ORIENTED_EDGE('',*,*,#1099,.F.);
#1387=ORIENTED_EDGE('',*,*,#1100,.T.);
#1388=ORIENTED_EDGE('',*,*,#988,.T.);
#1389=ORIENTED_EDGE('',*,*,#1101,.T.);
#1390=ORIENTED_EDGE('',*,*,#1102,.T.);
#1391=ORIENTED_EDGE('',*,*,#1097,.T.);
#1392=ORIENTED_EDGE('',*,*,#1011,.T.);
#1393=ORIENTED_EDGE('',*,*,#1100,.F.);
#1394=ORIENTED_EDGE('',*,*,#1103,.F.);
#1395=ORIENTED_EDGE('',*,*,#1039,.F.);
#1396=ORIENTED_EDGE('',*,*,#987,.T.);
#1397=ORIENTED_EDGE('',*,*,#1055,.F.);
#1398=ORIENTED_EDGE('',*,*,#1104,.F.);
#1399=ORIENTED_EDGE('',*,*,#1101,.F.);
#1400=ORIENTED_EDGE('',*,*,#1005,.T.);
#1401=ORIENTED_EDGE('',*,*,#1041,.T.);
#1402=ORIENTED_EDGE('',*,*,#1105,.F.);
#1403=ORIENTED_EDGE('',*,*,#1106,.F.);
#1404=ORIENTED_EDGE('',*,*,#989,.T.);
#1405=ORIENTED_EDGE('',*,*,#1107,.F.);
#1406=ORIENTED_EDGE('',*,*,#1108,.F.);
#1407=ORIENTED_EDGE('',*,*,#1053,.T.);
#1408=ORIENTED_EDGE('',*,*,#1006,.T.);
#1409=ORIENTED_EDGE('',*,*,#1106,.T.);
#1410=ORIENTED_EDGE('',*,*,#1109,.F.);
#1411=ORIENTED_EDGE('',*,*,#1110,.T.);
#1412=ORIENTED_EDGE('',*,*,#992,.T.);
#1413=ORIENTED_EDGE('',*,*,#1111,.T.);
#1414=ORIENTED_EDGE('',*,*,#1112,.T.);
#1415=ORIENTED_EDGE('',*,*,#1107,.T.);
#1416=ORIENTED_EDGE('',*,*,#1007,.T.);
#1417=ORIENTED_EDGE('',*,*,#1110,.F.);
#1418=ORIENTED_EDGE('',*,*,#1113,.F.);
#1419=ORIENTED_EDGE('',*,*,#1042,.F.);
#1420=ORIENTED_EDGE('',*,*,#991,.T.);
#1421=ORIENTED_EDGE('',*,*,#1052,.F.);
#1422=ORIENTED_EDGE('',*,*,#1114,.F.);
#1423=ORIENTED_EDGE('',*,*,#1111,.F.);
#1424=ORIENTED_EDGE('',*,*,#1001,.T.);
#1425=ORIENTED_EDGE('',*,*,#1044,.T.);
#1426=ORIENTED_EDGE('',*,*,#1115,.F.);
#1427=ORIENTED_EDGE('',*,*,#1116,.F.);
#1428=ORIENTED_EDGE('',*,*,#993,.T.);
#1429=ORIENTED_EDGE('',*,*,#1117,.F.);
#1430=ORIENTED_EDGE('',*,*,#1118,.F.);
#1431=ORIENTED_EDGE('',*,*,#1050,.T.);
#1432=ORIENTED_EDGE('',*,*,#1002,.T.);
#1433=ORIENTED_EDGE('',*,*,#1116,.T.);
#1434=ORIENTED_EDGE('',*,*,#1119,.F.);
#1435=ORIENTED_EDGE('',*,*,#1120,.T.);
#1436=ORIENTED_EDGE('',*,*,#996,.T.);
#1437=ORIENTED_EDGE('',*,*,#1121,.T.);
#1438=ORIENTED_EDGE('',*,*,#1122,.T.);
#1439=ORIENTED_EDGE('',*,*,#1117,.T.);
#1440=ORIENTED_EDGE('',*,*,#1003,.T.);
#1441=ORIENTED_EDGE('',*,*,#1120,.F.);
#1442=ORIENTED_EDGE('',*,*,#1123,.F.);
#1443=ORIENTED_EDGE('',*,*,#1045,.F.);
#1444=ORIENTED_EDGE('',*,*,#995,.T.);
#1445=ORIENTED_EDGE('',*,*,#1049,.F.);
#1446=ORIENTED_EDGE('',*,*,#1124,.F.);
#1447=ORIENTED_EDGE('',*,*,#1121,.F.);
#1448=ORIENTED_EDGE('',*,*,#1074,.T.);
#1449=ORIENTED_EDGE('',*,*,#1063,.T.);
#1450=ORIENTED_EDGE('',*,*,#1078,.T.);
#1451=ORIENTED_EDGE('',*,*,#1082,.F.);
#1452=ORIENTED_EDGE('',*,*,#1084,.T.);
#1453=ORIENTED_EDGE('',*,*,#1060,.T.);
#1454=ORIENTED_EDGE('',*,*,#1088,.T.);
#1455=ORIENTED_EDGE('',*,*,#1092,.F.);
#1456=ORIENTED_EDGE('',*,*,#1094,.T.);
#1457=ORIENTED_EDGE('',*,*,#1057,.T.);
#1458=ORIENTED_EDGE('',*,*,#1098,.T.);
#1459=ORIENTED_EDGE('',*,*,#1102,.F.);
#1460=ORIENTED_EDGE('',*,*,#1104,.T.);
#1461=ORIENTED_EDGE('',*,*,#1054,.T.);
#1462=ORIENTED_EDGE('',*,*,#1108,.T.);
#1463=ORIENTED_EDGE('',*,*,#1112,.F.);
#1464=ORIENTED_EDGE('',*,*,#1114,.T.);
#1465=ORIENTED_EDGE('',*,*,#1051,.T.);
#1466=ORIENTED_EDGE('',*,*,#1118,.T.);
#1467=ORIENTED_EDGE('',*,*,#1122,.F.);
#1468=ORIENTED_EDGE('',*,*,#1124,.T.);
#1469=ORIENTED_EDGE('',*,*,#1048,.T.);
#1470=ORIENTED_EDGE('',*,*,#1125,.T.);
#1471=ORIENTED_EDGE('',*,*,#1126,.T.);
#1472=ORIENTED_EDGE('',*,*,#1127,.F.);
#1473=ORIENTED_EDGE('',*,*,#1026,.T.);
#1474=ORIENTED_EDGE('',*,*,#1068,.T.);
#1475=ORIENTED_EDGE('',*,*,#1072,.F.);
#1476=ORIENTED_EDGE('',*,*,#1047,.T.);
#1477=ORIENTED_EDGE('',*,*,#1128,.F.);
#1478=ORIENTED_EDGE('',*,*,#1129,.F.);
#1479=ORIENTED_EDGE('',*,*,#1125,.F.);
#1480=ORIENTED_EDGE('',*,*,#1073,.T.);
#1481=ORIENTED_EDGE('',*,*,#1069,.T.);
#1482=ORIENTED_EDGE('',*,*,#1065,.T.);
#1483=ORIENTED_EDGE('',*,*,#1028,.T.);
#1484=ORIENTED_EDGE('',*,*,#1130,.F.);
#1485=ORIENTED_EDGE('',*,*,#1131,.F.);
#1486=ORIENTED_EDGE('',*,*,#1128,.T.);
#1487=ORIENTED_EDGE('',*,*,#1046,.T.);
#1488=ORIENTED_EDGE('',*,*,#1123,.T.);
#1489=ORIENTED_EDGE('',*,*,#1119,.T.);
#1490=ORIENTED_EDGE('',*,*,#1115,.T.);
#1491=ORIENTED_EDGE('',*,*,#1043,.T.);
#1492=ORIENTED_EDGE('',*,*,#1113,.T.);
#1493=ORIENTED_EDGE('',*,*,#1109,.T.);
#1494=ORIENTED_EDGE('',*,*,#1105,.T.);
#1495=ORIENTED_EDGE('',*,*,#1040,.T.);
#1496=ORIENTED_EDGE('',*,*,#1103,.T.);
#1497=ORIENTED_EDGE('',*,*,#1099,.T.);
#1498=ORIENTED_EDGE('',*,*,#1095,.T.);
#1499=ORIENTED_EDGE('',*,*,#1037,.T.);
#1500=ORIENTED_EDGE('',*,*,#1093,.T.);
#1501=ORIENTED_EDGE('',*,*,#1089,.T.);
#1502=ORIENTED_EDGE('',*,*,#1085,.T.);
#1503=ORIENTED_EDGE('',*,*,#1034,.T.);
#1504=ORIENTED_EDGE('',*,*,#1083,.T.);
#1505=ORIENTED_EDGE('',*,*,#1079,.T.);
#1506=ORIENTED_EDGE('',*,*,#1075,.T.);
#1507=ORIENTED_EDGE('',*,*,#1031,.T.);
#1508=ORIENTED_EDGE('',*,*,#1129,.T.);
#1509=ORIENTED_EDGE('',*,*,#1131,.T.);
#1510=ORIENTED_EDGE('',*,*,#1132,.F.);
#1511=ORIENTED_EDGE('',*,*,#1126,.F.);
#1512=ORIENTED_EDGE('',*,*,#965,.T.);
#1513=ORIENTED_EDGE('',*,*,#968,.T.);
#1514=ORIENTED_EDGE('',*,*,#971,.T.);
#1515=ORIENTED_EDGE('',*,*,#974,.T.);
#1516=ORIENTED_EDGE('',*,*,#1027,.T.);
#1517=ORIENTED_EDGE('',*,*,#1127,.T.);
#1518=ORIENTED_EDGE('',*,*,#1132,.T.);
#1519=ORIENTED_EDGE('',*,*,#1130,.T.);
#1520=ORIENTED_EDGE('',*,*,#1133,.F.);
#1521=ORIENTED_EDGE('',*,*,#1134,.F.);
#1522=ORIENTED_EDGE('',*,*,#1135,.F.);
#1523=ORIENTED_EDGE('',*,*,#1136,.F.);
#1524=ORIENTED_EDGE('',*,*,#1137,.F.);
#1525=ORIENTED_EDGE('',*,*,#1138,.F.);
#1526=ORIENTED_EDGE('',*,*,#1139,.F.);
#1527=ORIENTED_EDGE('',*,*,#1140,.F.);
#1528=ORIENTED_EDGE('',*,*,#1141,.F.);
#1529=ORIENTED_EDGE('',*,*,#1135,.T.);
#1530=ORIENTED_EDGE('',*,*,#1142,.F.);
#1531=ORIENTED_EDGE('',*,*,#1139,.T.);
#1532=ORIENTED_EDGE('',*,*,#1140,.T.);
#1533=ORIENTED_EDGE('',*,*,#1142,.T.);
#1534=ORIENTED_EDGE('',*,*,#1134,.T.);
#1535=ORIENTED_EDGE('',*,*,#1143,.F.);
#1536=ORIENTED_EDGE('',*,*,#1144,.F.);
#1537=ORIENTED_EDGE('',*,*,#1145,.T.);
#1538=ORIENTED_EDGE('',*,*,#1146,.T.);
#1539=ORIENTED_EDGE('',*,*,#1147,.F.);
#1540=ORIENTED_EDGE('',*,*,#1133,.T.);
#1541=ORIENTED_EDGE('',*,*,#1148,.T.);
#1542=ORIENTED_EDGE('',*,*,#1149,.T.);
#1543=ORIENTED_EDGE('',*,*,#1143,.T.);
#1544=ORIENTED_EDGE('',*,*,#1150,.T.);
#1545=ORIENTED_EDGE('',*,*,#1151,.T.);
#1546=ORIENTED_EDGE('',*,*,#1152,.F.);
#1547=ORIENTED_EDGE('',*,*,#1146,.F.);
#1548=ORIENTED_EDGE('',*,*,#1153,.T.);
#1549=ORIENTED_EDGE('',*,*,#1144,.T.);
#1550=ORIENTED_EDGE('',*,*,#1149,.F.);
#1551=ORIENTED_EDGE('',*,*,#1154,.F.);
#1552=ORIENTED_EDGE('',*,*,#1138,.T.);
#1553=ORIENTED_EDGE('',*,*,#1155,.F.);
#1554=ORIENTED_EDGE('',*,*,#1151,.F.);
#1555=ORIENTED_EDGE('',*,*,#1156,.T.);
#1556=ORIENTED_EDGE('',*,*,#1154,.T.);
#1557=ORIENTED_EDGE('',*,*,#1148,.F.);
#1558=ORIENTED_EDGE('',*,*,#1136,.T.);
#1559=ORIENTED_EDGE('',*,*,#1141,.T.);
#1560=ORIENTED_EDGE('',*,*,#1137,.T.);
#1561=ORIENTED_EDGE('',*,*,#1147,.T.);
#1562=ORIENTED_EDGE('',*,*,#1152,.T.);
#1563=ORIENTED_EDGE('',*,*,#1155,.T.);
#1564=ORIENTED_EDGE('',*,*,#1156,.F.);
#1565=ORIENTED_EDGE('',*,*,#1150,.F.);
#1566=ORIENTED_EDGE('',*,*,#1145,.F.);
#1567=ORIENTED_EDGE('',*,*,#1153,.F.);
#1568=ORIENTED_EDGE('',*,*,#1157,.T.);
#1569=ORIENTED_EDGE('',*,*,#1158,.T.);
#1570=ORIENTED_EDGE('',*,*,#1159,.F.);
#1571=ORIENTED_EDGE('',*,*,#1160,.F.);
#1572=ORIENTED_EDGE('',*,*,#1161,.T.);
#1573=ORIENTED_EDGE('',*,*,#1160,.T.);
#1574=ORIENTED_EDGE('',*,*,#1162,.F.);
#1575=ORIENTED_EDGE('',*,*,#1163,.F.);
#1576=ORIENTED_EDGE('',*,*,#1164,.T.);
#1577=ORIENTED_EDGE('',*,*,#1163,.T.);
#1578=ORIENTED_EDGE('',*,*,#1165,.F.);
#1579=ORIENTED_EDGE('',*,*,#1166,.F.);
#1580=ORIENTED_EDGE('',*,*,#1167,.T.);
#1581=ORIENTED_EDGE('',*,*,#1166,.T.);
#1582=ORIENTED_EDGE('',*,*,#1168,.F.);
#1583=ORIENTED_EDGE('',*,*,#1158,.F.);
#1584=ORIENTED_EDGE('',*,*,#1168,.T.);
#1585=ORIENTED_EDGE('',*,*,#1165,.T.);
#1586=ORIENTED_EDGE('',*,*,#1162,.T.);
#1587=ORIENTED_EDGE('',*,*,#1159,.T.);
#1588=ORIENTED_EDGE('',*,*,#1167,.F.);
#1589=ORIENTED_EDGE('',*,*,#1157,.F.);
#1590=ORIENTED_EDGE('',*,*,#1161,.F.);
#1591=ORIENTED_EDGE('',*,*,#1164,.F.);
#1592=ORIENTED_EDGE('',*,*,#1169,.T.);
#1593=ORIENTED_EDGE('',*,*,#1170,.T.);
#1594=ORIENTED_EDGE('',*,*,#1171,.F.);
#1595=ORIENTED_EDGE('',*,*,#1172,.F.);
#1596=ORIENTED_EDGE('',*,*,#1173,.T.);
#1597=ORIENTED_EDGE('',*,*,#1172,.T.);
#1598=ORIENTED_EDGE('',*,*,#1174,.F.);
#1599=ORIENTED_EDGE('',*,*,#1175,.F.);
#1600=ORIENTED_EDGE('',*,*,#1176,.T.);
#1601=ORIENTED_EDGE('',*,*,#1175,.T.);
#1602=ORIENTED_EDGE('',*,*,#1177,.F.);
#1603=ORIENTED_EDGE('',*,*,#1178,.F.);
#1604=ORIENTED_EDGE('',*,*,#1179,.T.);
#1605=ORIENTED_EDGE('',*,*,#1178,.T.);
#1606=ORIENTED_EDGE('',*,*,#1180,.F.);
#1607=ORIENTED_EDGE('',*,*,#1170,.F.);
#1608=ORIENTED_EDGE('',*,*,#1180,.T.);
#1609=ORIENTED_EDGE('',*,*,#1177,.T.);
#1610=ORIENTED_EDGE('',*,*,#1174,.T.);
#1611=ORIENTED_EDGE('',*,*,#1171,.T.);
#1612=ORIENTED_EDGE('',*,*,#1179,.F.);
#1613=ORIENTED_EDGE('',*,*,#1169,.F.);
#1614=ORIENTED_EDGE('',*,*,#1173,.F.);
#1615=ORIENTED_EDGE('',*,*,#1176,.F.);
#1616=ORIENTED_EDGE('',*,*,#1181,.F.);
#1617=ORIENTED_EDGE('',*,*,#1182,.T.);
#1618=ORIENTED_EDGE('',*,*,#1183,.T.);
#1619=ORIENTED_EDGE('',*,*,#1182,.F.);
#1620=ORIENTED_EDGE('',*,*,#1181,.T.);
#1621=ORIENTED_EDGE('',*,*,#1183,.F.);
#1622=CYLINDRICAL_SURFACE('',#1777,0.409999999999997);
#1623=CYLINDRICAL_SURFACE('',#1781,0.409999999999997);
#1624=CYLINDRICAL_SURFACE('',#1785,0.409999999999997);
#1625=CYLINDRICAL_SURFACE('',#1789,0.409999999999997);
#1626=CYLINDRICAL_SURFACE('',#1873,0.4);
#1627=ADVANCED_FACE('',(#213),#1622,.F.);
#1628=ADVANCED_FACE('',(#214),#131,.F.);
#1629=ADVANCED_FACE('',(#215),#1623,.F.);
#1630=ADVANCED_FACE('',(#216),#132,.F.);
#1631=ADVANCED_FACE('',(#217),#1624,.F.);
#1632=ADVANCED_FACE('',(#218),#133,.F.);
#1633=ADVANCED_FACE('',(#219),#1625,.F.);
#1634=ADVANCED_FACE('',(#220),#134,.F.);
#1635=ADVANCED_FACE('',(#221),#135,.F.);
#1636=ADVANCED_FACE('',(#222),#136,.F.);
#1637=ADVANCED_FACE('',(#223),#137,.F.);
#1638=ADVANCED_FACE('',(#224),#138,.F.);
#1639=ADVANCED_FACE('',(#225),#139,.F.);
#1640=ADVANCED_FACE('',(#226),#140,.F.);
#1641=ADVANCED_FACE('',(#227),#141,.F.);
#1642=ADVANCED_FACE('',(#228),#142,.F.);
#1643=ADVANCED_FACE('',(#229),#143,.F.);
#1644=ADVANCED_FACE('',(#230),#144,.F.);
#1645=ADVANCED_FACE('',(#231),#145,.F.);
#1646=ADVANCED_FACE('',(#232),#146,.F.);
#1647=ADVANCED_FACE('',(#233),#147,.F.);
#1648=ADVANCED_FACE('',(#234),#148,.T.);
#1649=ADVANCED_FACE('',(#235),#149,.T.);
#1650=ADVANCED_FACE('',(#236),#150,.T.);
#1651=ADVANCED_FACE('',(#237),#151,.T.);
#1652=ADVANCED_FACE('',(#238),#152,.F.);
#1653=ADVANCED_FACE('',(#239),#153,.F.);
#1654=ADVANCED_FACE('',(#240),#154,.T.);
#1655=ADVANCED_FACE('',(#241),#155,.T.);
#1656=ADVANCED_FACE('',(#242),#156,.T.);
#1657=ADVANCED_FACE('',(#243),#157,.T.);
#1658=ADVANCED_FACE('',(#244),#158,.F.);
#1659=ADVANCED_FACE('',(#245),#159,.F.);
#1660=ADVANCED_FACE('',(#246),#160,.T.);
#1661=ADVANCED_FACE('',(#247),#161,.T.);
#1662=ADVANCED_FACE('',(#248),#162,.T.);
#1663=ADVANCED_FACE('',(#249),#163,.T.);
#1664=ADVANCED_FACE('',(#250),#164,.F.);
#1665=ADVANCED_FACE('',(#251),#165,.F.);
#1666=ADVANCED_FACE('',(#252),#166,.T.);
#1667=ADVANCED_FACE('',(#253),#167,.T.);
#1668=ADVANCED_FACE('',(#254),#168,.T.);
#1669=ADVANCED_FACE('',(#255),#169,.T.);
#1670=ADVANCED_FACE('',(#256),#170,.F.);
#1671=ADVANCED_FACE('',(#257),#171,.F.);
#1672=ADVANCED_FACE('',(#258),#172,.T.);
#1673=ADVANCED_FACE('',(#259),#173,.T.);
#1674=ADVANCED_FACE('',(#260),#174,.T.);
#1675=ADVANCED_FACE('',(#261),#175,.T.);
#1676=ADVANCED_FACE('',(#262),#176,.F.);
#1677=ADVANCED_FACE('',(#263),#177,.F.);
#1678=ADVANCED_FACE('',(#264),#178,.T.);
#1679=ADVANCED_FACE('',(#265),#179,.T.);
#1680=ADVANCED_FACE('',(#266),#180,.T.);
#1681=ADVANCED_FACE('',(#267),#181,.T.);
#1682=ADVANCED_FACE('',(#268),#182,.F.);
#1683=ADVANCED_FACE('',(#269),#183,.F.);
#1684=ADVANCED_FACE('',(#270),#184,.T.);
#1685=ADVANCED_FACE('',(#271),#185,.F.);
#1686=ADVANCED_FACE('',(#272),#186,.T.);
#1687=ADVANCED_FACE('',(#273,#127,#128,#129,#130),#187,.T.);
#1688=ADVANCED_FACE('',(#274),#188,.T.);
#1689=ADVANCED_FACE('',(#275),#189,.F.);
#1690=ADVANCED_FACE('',(#276),#190,.F.);
#1691=ADVANCED_FACE('',(#277),#191,.T.);
#1692=ADVANCED_FACE('',(#278),#192,.T.);
#1693=ADVANCED_FACE('',(#279),#193,.T.);
#1694=ADVANCED_FACE('',(#280),#194,.T.);
#1695=ADVANCED_FACE('',(#281),#195,.T.);
#1696=ADVANCED_FACE('',(#282),#196,.T.);
#1697=ADVANCED_FACE('',(#283),#197,.T.);
#1698=ADVANCED_FACE('',(#284),#198,.F.);
#1699=ADVANCED_FACE('',(#285),#199,.T.);
#1700=ADVANCED_FACE('',(#286),#200,.T.);
#1701=ADVANCED_FACE('',(#287),#201,.T.);
#1702=ADVANCED_FACE('',(#288),#202,.T.);
#1703=ADVANCED_FACE('',(#289),#203,.T.);
#1704=ADVANCED_FACE('',(#290),#204,.F.);
#1705=ADVANCED_FACE('',(#291),#205,.T.);
#1706=ADVANCED_FACE('',(#292),#206,.T.);
#1707=ADVANCED_FACE('',(#293),#207,.T.);
#1708=ADVANCED_FACE('',(#294),#208,.T.);
#1709=ADVANCED_FACE('',(#295),#209,.T.);
#1710=ADVANCED_FACE('',(#296),#210,.F.);
#1711=ADVANCED_FACE('',(#297),#1626,.T.);
#1712=ADVANCED_FACE('',(#298),#211,.T.);
#1713=ADVANCED_FACE('',(#299),#212,.F.);
#1714=CLOSED_SHELL('',(#1627,#1628,#1629,#1630,#1631,#1632,#1633,#1634,
#1635,#1636,#1637,#1638,#1639,#1640,#1641,#1642,#1643,#1644,#1645,#1646,
#1647,#1648,#1649,#1650,#1651,#1652,#1653,#1654,#1655,#1656,#1657,#1658,
#1659,#1660,#1661,#1662,#1663,#1664,#1665,#1666,#1667,#1668,#1669,#1670,
#1671,#1672,#1673,#1674,#1675,#1676,#1677,#1678,#1679,#1680,#1681,#1682,
#1683,#1684,#1685,#1686,#1687,#1688));
#1715=CLOSED_SHELL('',(#1689,#1690,#1691,#1692,#1693,#1694,#1695,#1696,
#1697,#1698));
#1716=CLOSED_SHELL('',(#1699,#1700,#1701,#1702,#1703,#1704));
#1717=CLOSED_SHELL('',(#1705,#1706,#1707,#1708,#1709,#1710));
#1718=CLOSED_SHELL('',(#1711,#1712,#1713));
#1719=DERIVED_UNIT_ELEMENT(#1729,1.);
#1720=DERIVED_UNIT_ELEMENT(#2862,-3.);
#1721=DERIVED_UNIT_ELEMENT(#1729,1.);
#1722=DERIVED_UNIT_ELEMENT(#2862,-3.);
#1723=DERIVED_UNIT_ELEMENT(#1729,1.);
#1724=DERIVED_UNIT_ELEMENT(#2862,-3.);
#1725=DERIVED_UNIT_ELEMENT(#1729,1.);
#1726=DERIVED_UNIT_ELEMENT(#2862,-3.);
#1727=DERIVED_UNIT_ELEMENT(#1729,1.);
#1728=DERIVED_UNIT_ELEMENT(#2862,-3.);
#1729=(
MASS_UNIT()
NAMED_UNIT(*)
SI_UNIT(.KILO.,.GRAM.)
);
#1730=DERIVED_UNIT((#1719,#1720));
#1731=DERIVED_UNIT((#1721,#1722));
#1732=DERIVED_UNIT((#1723,#1724));
#1733=DERIVED_UNIT((#1725,#1726));
#1734=DERIVED_UNIT((#1727,#1728));
#1735=MEASURE_REPRESENTATION_ITEM('density measure',
POSITIVE_RATIO_MEASURE(7850.),#1730);
#1736=MEASURE_REPRESENTATION_ITEM('density measure',
POSITIVE_RATIO_MEASURE(7850.),#1731);
#1737=MEASURE_REPRESENTATION_ITEM('density measure',
POSITIVE_RATIO_MEASURE(7850.),#1732);
#1738=MEASURE_REPRESENTATION_ITEM('density measure',
POSITIVE_RATIO_MEASURE(7850.),#1733);
#1739=MEASURE_REPRESENTATION_ITEM('density measure',
POSITIVE_RATIO_MEASURE(7850.),#1734);
#1740=PROPERTY_DEFINITION_REPRESENTATION(#1765,#1750);
#1741=PROPERTY_DEFINITION_REPRESENTATION(#1766,#1751);
#1742=PROPERTY_DEFINITION_REPRESENTATION(#1767,#1752);
#1743=PROPERTY_DEFINITION_REPRESENTATION(#1768,#1753);
#1744=PROPERTY_DEFINITION_REPRESENTATION(#1769,#1754);
#1745=PROPERTY_DEFINITION_REPRESENTATION(#1770,#1755);
#1746=PROPERTY_DEFINITION_REPRESENTATION(#1771,#1756);
#1747=PROPERTY_DEFINITION_REPRESENTATION(#1772,#1757);
#1748=PROPERTY_DEFINITION_REPRESENTATION(#1773,#1758);
#1749=PROPERTY_DEFINITION_REPRESENTATION(#1774,#1759);
#1750=REPRESENTATION('material name',(#1760),#2855);
#1751=REPRESENTATION('density',(#1735),#2855);
#1752=REPRESENTATION('material name',(#1761),#2856);
#1753=REPRESENTATION('density',(#1736),#2856);
#1754=REPRESENTATION('material name',(#1762),#2857);
#1755=REPRESENTATION('density',(#1737),#2857);
#1756=REPRESENTATION('material name',(#1763),#2858);
#1757=REPRESENTATION('density',(#1738),#2858);
#1758=REPRESENTATION('material name',(#1764),#2859);
#1759=REPRESENTATION('density',(#1739),#2859);
#1760=DESCRIPTIVE_REPRESENTATION_ITEM('Steel','Steel');
#1761=DESCRIPTIVE_REPRESENTATION_ITEM('Steel','Steel');
#1762=DESCRIPTIVE_REPRESENTATION_ITEM('Steel','Steel');
#1763=DESCRIPTIVE_REPRESENTATION_ITEM('Steel','Steel');
#1764=DESCRIPTIVE_REPRESENTATION_ITEM('Steel','Steel');
#1765=PROPERTY_DEFINITION('material property','material name',#2909);
#1766=PROPERTY_DEFINITION('material property','density of part',#2909);
#1767=PROPERTY_DEFINITION('material property','material name',#2910);
#1768=PROPERTY_DEFINITION('material property','density of part',#2910);
#1769=PROPERTY_DEFINITION('material property','material name',#2911);
#1770=PROPERTY_DEFINITION('material property','density of part',#2911);
#1771=PROPERTY_DEFINITION('material property','material name',#2912);
#1772=PROPERTY_DEFINITION('material property','density of part',#2912);
#1773=PROPERTY_DEFINITION('material property','material name',#2913);
#1774=PROPERTY_DEFINITION('material property','density of part',#2913);
#1775=AXIS2_PLACEMENT_3D('',#2365,#1902,#1903);
#1776=AXIS2_PLACEMENT_3D('',#2366,#1904,#1905);
#1777=AXIS2_PLACEMENT_3D('',#2367,#1906,#1907);
#1778=AXIS2_PLACEMENT_3D('',#2369,#1908,#1909);
#1779=AXIS2_PLACEMENT_3D('',#2372,#1911,#1912);
#1780=AXIS2_PLACEMENT_3D('',#2373,#1913,#1914);
#1781=AXIS2_PLACEMENT_3D('',#2374,#1915,#1916);
#1782=AXIS2_PLACEMENT_3D('',#2376,#1917,#1918);
#1783=AXIS2_PLACEMENT_3D('',#2379,#1920,#1921);
#1784=AXIS2_PLACEMENT_3D('',#2380,#1922,#1923);
#1785=AXIS2_PLACEMENT_3D('',#2381,#1924,#1925);
#1786=AXIS2_PLACEMENT_3D('',#2383,#1926,#1927);
#1787=AXIS2_PLACEMENT_3D('',#2386,#1929,#1930);
#1788=AXIS2_PLACEMENT_3D('',#2387,#1931,#1932);
#1789=AXIS2_PLACEMENT_3D('',#2388,#1933,#1934);
#1790=AXIS2_PLACEMENT_3D('',#2390,#1935,#1936);
#1791=AXIS2_PLACEMENT_3D('',#2393,#1938,#1939);
#1792=AXIS2_PLACEMENT_3D('',#2394,#1940,#1941);
#1793=AXIS2_PLACEMENT_3D('',#2395,#1942,#1943);
#1794=AXIS2_PLACEMENT_3D('',#2404,#1948,#1949);
#1795=AXIS2_PLACEMENT_3D('',#2413,#1954,#1955);
#1796=AXIS2_PLACEMENT_3D('',#2422,#1960,#1961);
#1797=AXIS2_PLACEMENT_3D('',#2431,#1966,#1967);
#1798=AXIS2_PLACEMENT_3D('',#2440,#1972,#1973);
#1799=AXIS2_PLACEMENT_3D('',#2449,#1978,#1979);
#1800=AXIS2_PLACEMENT_3D('',#2458,#1984,#1985);
#1801=AXIS2_PLACEMENT_3D('',#2467,#1990,#1991);
#1802=AXIS2_PLACEMENT_3D('',#2476,#1996,#1997);
#1803=AXIS2_PLACEMENT_3D('',#2485,#2002,#2003);
#1804=AXIS2_PLACEMENT_3D('',#2494,#2008,#2009);
#1805=AXIS2_PLACEMENT_3D('',#2503,#2014,#2015);
#1806=AXIS2_PLACEMENT_3D('',#2572,#2056,#2057);
#1807=AXIS2_PLACEMENT_3D('',#2576,#2060,#2061);
#1808=AXIS2_PLACEMENT_3D('',#2580,#2064,#2065);
#1809=AXIS2_PLACEMENT_3D('',#2584,#2068,#2069);
#1810=AXIS2_PLACEMENT_3D('',#2588,#2072,#2073);
#1811=AXIS2_PLACEMENT_3D('',#2590,#2075,#2076);
#1812=AXIS2_PLACEMENT_3D('',#2592,#2078,#2079);
#1813=AXIS2_PLACEMENT_3D('',#2596,#2082,#2083);
#1814=AXIS2_PLACEMENT_3D('',#2600,#2086,#2087);
#1815=AXIS2_PLACEMENT_3D('',#2604,#2090,#2091);
#1816=AXIS2_PLACEMENT_3D('',#2608,#2094,#2095);
#1817=AXIS2_PLACEMENT_3D('',#2610,#2097,#2098);
#1818=AXIS2_PLACEMENT_3D('',#2612,#2100,#2101);
#1819=AXIS2_PLACEMENT_3D('',#2616,#2104,#2105);
#1820=AXIS2_PLACEMENT_3D('',#2620,#2108,#2109);
#1821=AXIS2_PLACEMENT_3D('',#2624,#2112,#2113);
#1822=AXIS2_PLACEMENT_3D('',#2628,#2116,#2117);
#1823=AXIS2_PLACEMENT_3D('',#2630,#2119,#2120);
#1824=AXIS2_PLACEMENT_3D('',#2632,#2122,#2123);
#1825=AXIS2_PLACEMENT_3D('',#2636,#2126,#2127);
#1826=AXIS2_PLACEMENT_3D('',#2640,#2130,#2131);
#1827=AXIS2_PLACEMENT_3D('',#2644,#2134,#2135);
#1828=AXIS2_PLACEMENT_3D('',#2648,#2138,#2139);
#1829=AXIS2_PLACEMENT_3D('',#2650,#2141,#2142);
#1830=AXIS2_PLACEMENT_3D('',#2652,#2144,#2145);
#1831=AXIS2_PLACEMENT_3D('',#2656,#2148,#2149);
#1832=AXIS2_PLACEMENT_3D('',#2660,#2152,#2153);
#1833=AXIS2_PLACEMENT_3D('',#2664,#2156,#2157);
#1834=AXIS2_PLACEMENT_3D('',#2668,#2160,#2161);
#1835=AXIS2_PLACEMENT_3D('',#2670,#2163,#2164);
#1836=AXIS2_PLACEMENT_3D('',#2672,#2166,#2167);
#1837=AXIS2_PLACEMENT_3D('',#2676,#2170,#2171);
#1838=AXIS2_PLACEMENT_3D('',#2680,#2174,#2175);
#1839=AXIS2_PLACEMENT_3D('',#2684,#2178,#2179);
#1840=AXIS2_PLACEMENT_3D('',#2688,#2182,#2183);
#1841=AXIS2_PLACEMENT_3D('',#2690,#2185,#2186);
#1842=AXIS2_PLACEMENT_3D('',#2692,#2188,#2189);
#1843=AXIS2_PLACEMENT_3D('',#2698,#2193,#2194);
#1844=AXIS2_PLACEMENT_3D('',#2702,#2197,#2198);
#1845=AXIS2_PLACEMENT_3D('',#2706,#2201,#2202);
#1846=AXIS2_PLACEMENT_3D('',#2708,#2204,#2205);
#1847=AXIS2_PLACEMENT_3D('',#2709,#2206,#2207);
#1848=AXIS2_PLACEMENT_3D('',#2710,#2208,#2209);
#1849=AXIS2_PLACEMENT_3D('',#2719,#2214,#2215);
#1850=AXIS2_PLACEMENT_3D('',#2728,#2220,#2221);
#1851=AXIS2_PLACEMENT_3D('',#2731,#2224,#2225);
#1852=AXIS2_PLACEMENT_3D('',#2741,#2231,#2232);
#1853=AXIS2_PLACEMENT_3D('',#2745,#2235,#2236);
#1854=AXIS2_PLACEMENT_3D('',#2751,#2240,#2241);
#1855=AXIS2_PLACEMENT_3D('',#2755,#2244,#2245);
#1856=AXIS2_PLACEMENT_3D('',#2758,#2248,#2249);
#1857=AXIS2_PLACEMENT_3D('',#2759,#2250,#2251);
#1858=AXIS2_PLACEMENT_3D('',#2760,#2252,#2253);
#1859=AXIS2_PLACEMENT_3D('',#2761,#2254,#2255);
#1860=AXIS2_PLACEMENT_3D('',#2770,#2260,#2261);
#1861=AXIS2_PLACEMENT_3D('',#2776,#2265,#2266);
#1862=AXIS2_PLACEMENT_3D('',#2782,#2270,#2271);
#1863=AXIS2_PLACEMENT_3D('',#2785,#2274,#2275);
#1864=AXIS2_PLACEMENT_3D('',#2786,#2276,#2277);
#1865=AXIS2_PLACEMENT_3D('',#2787,#2278,#2279);
#1866=AXIS2_PLACEMENT_3D('',#2788,#2280,#2281);
#1867=AXIS2_PLACEMENT_3D('',#2797,#2286,#2287);
#1868=AXIS2_PLACEMENT_3D('',#2803,#2291,#2292);
#1869=AXIS2_PLACEMENT_3D('',#2809,#2296,#2297);
#1870=AXIS2_PLACEMENT_3D('',#2812,#2300,#2301);
#1871=AXIS2_PLACEMENT_3D('',#2813,#2302,#2303);
#1872=AXIS2_PLACEMENT_3D('',#2814,#2304,#2305);
#1873=AXIS2_PLACEMENT_3D('',#2815,#2306,#2307);
#1874=AXIS2_PLACEMENT_3D('',#2817,#2308,#2309);
#1875=AXIS2_PLACEMENT_3D('',#2820,#2311,#2312);
#1876=AXIS2_PLACEMENT_3D('',#2821,#2313,#2314);
#1877=AXIS2_PLACEMENT_3D('',#2822,#2315,#2316);
#1878=AXIS2_PLACEMENT_3D('',#2823,#2317,#2318);
#1879=AXIS2_PLACEMENT_3D('',#2824,#2319,#2320);
#1880=AXIS2_PLACEMENT_3D('',#2825,#2321,#2322);
#1881=AXIS2_PLACEMENT_3D('',#2826,#2323,#2324);
#1882=AXIS2_PLACEMENT_3D('',#2827,#2325,#2326);
#1883=AXIS2_PLACEMENT_3D('',#2828,#2327,#2328);
#1884=AXIS2_PLACEMENT_3D('',#2829,#2329,#2330);
#1885=AXIS2_PLACEMENT_3D('',#2830,#2331,#2332);
#1886=AXIS2_PLACEMENT_3D('',#2831,#2333,#2334);
#1887=AXIS2_PLACEMENT_3D('',#2832,#2335,#2336);
#1888=AXIS2_PLACEMENT_3D('',#2833,#2337,#2338);
#1889=AXIS2_PLACEMENT_3D('',#2834,#2339,#2340);
#1890=AXIS2_PLACEMENT_3D('',#2835,#2341,#2342);
#1891=AXIS2_PLACEMENT_3D('',#2836,#2343,#2344);
#1892=AXIS2_PLACEMENT_3D('',#2837,#2345,#2346);
#1893=AXIS2_PLACEMENT_3D('',#2838,#2347,#2348);
#1894=AXIS2_PLACEMENT_3D('',#2839,#2349,#2350);
#1895=AXIS2_PLACEMENT_3D('',#2840,#2351,#2352);
#1896=AXIS2_PLACEMENT_3D('',#2841,#2353,#2354);
#1897=AXIS2_PLACEMENT_3D('',#2842,#2355,#2356);
#1898=AXIS2_PLACEMENT_3D('',#2843,#2357,#2358);
#1899=AXIS2_PLACEMENT_3D('',#2844,#2359,#2360);
#1900=AXIS2_PLACEMENT_3D('',#2845,#2361,#2362);
#1901=AXIS2_PLACEMENT_3D('',#2846,#2363,#2364);
#1902=DIRECTION('axis',(0.,0.,1.));
#1903=DIRECTION('refdir',(1.,0.,0.));
#1904=DIRECTION('axis',(0.,0.,1.));
#1905=DIRECTION('refdir',(1.,0.,0.));
#1906=DIRECTION('center_axis',(1.,0.,0.));
#1907=DIRECTION('ref_axis',(0.,0.,-1.));
#1908=DIRECTION('center_axis',(1.,0.,0.));
#1909=DIRECTION('ref_axis',(0.,0.,-1.));
#1910=DIRECTION('',(1.,0.,0.));
#1911=DIRECTION('center_axis',(1.,0.,0.));
#1912=DIRECTION('ref_axis',(0.,0.,-1.));
#1913=DIRECTION('center_axis',(1.,0.,0.));
#1914=DIRECTION('ref_axis',(0.,0.,-1.));
#1915=DIRECTION('center_axis',(1.,0.,0.));
#1916=DIRECTION('ref_axis',(0.,0.,-1.));
#1917=DIRECTION('center_axis',(1.,0.,0.));
#1918=DIRECTION('ref_axis',(0.,0.,-1.));
#1919=DIRECTION('',(1.,0.,0.));
#1920=DIRECTION('center_axis',(1.,0.,0.));
#1921=DIRECTION('ref_axis',(0.,0.,-1.));
#1922=DIRECTION('center_axis',(1.,0.,0.));
#1923=DIRECTION('ref_axis',(0.,0.,-1.));
#1924=DIRECTION('center_axis',(1.,0.,0.));
#1925=DIRECTION('ref_axis',(0.,0.,-1.));
#1926=DIRECTION('center_axis',(1.,0.,0.));
#1927=DIRECTION('ref_axis',(0.,0.,-1.));
#1928=DIRECTION('',(1.,0.,0.));
#1929=DIRECTION('center_axis',(1.,0.,0.));
#1930=DIRECTION('ref_axis',(0.,0.,-1.));
#1931=DIRECTION('center_axis',(1.,0.,0.));
#1932=DIRECTION('ref_axis',(0.,0.,-1.));
#1933=DIRECTION('center_axis',(1.,0.,0.));
#1934=DIRECTION('ref_axis',(0.,0.,-1.));
#1935=DIRECTION('center_axis',(1.,0.,0.));
#1936=DIRECTION('ref_axis',(0.,0.,-1.));
#1937=DIRECTION('',(1.,0.,0.));
#1938=DIRECTION('center_axis',(1.,0.,0.));
#1939=DIRECTION('ref_axis',(0.,0.,-1.));
#1940=DIRECTION('center_axis',(1.,0.,0.));
#1941=DIRECTION('ref_axis',(0.,0.,-1.));
#1942=DIRECTION('center_axis',(0.,1.,0.));
#1943=DIRECTION('ref_axis',(-1.,0.,0.));
#1944=DIRECTION('',(1.,0.,0.));
#1945=DIRECTION('',(0.,0.,1.));
#1946=DIRECTION('',(-1.,0.,0.));
#1947=DIRECTION('',(0.,0.,-1.));
#1948=DIRECTION('center_axis',(0.,1.,0.));
#1949=DIRECTION('ref_axis',(-1.,0.,0.));
#1950=DIRECTION('',(1.,0.,0.));
#1951=DIRECTION('',(0.,0.,1.));
#1952=DIRECTION('',(-1.,0.,0.));
#1953=DIRECTION('',(0.,0.,-1.));
#1954=DIRECTION('center_axis',(0.,1.,0.));
#1955=DIRECTION('ref_axis',(-1.,0.,0.));
#1956=DIRECTION('',(1.,0.,0.));
#1957=DIRECTION('',(0.,0.,1.));
#1958=DIRECTION('',(-1.,0.,0.));
#1959=DIRECTION('',(0.,0.,-1.));
#1960=DIRECTION('center_axis',(0.,1.,0.));
#1961=DIRECTION('ref_axis',(-1.,0.,0.));
#1962=DIRECTION('',(1.,0.,0.));
#1963=DIRECTION('',(0.,0.,1.));
#1964=DIRECTION('',(-1.,0.,0.));
#1965=DIRECTION('',(0.,0.,-1.));
#1966=DIRECTION('center_axis',(0.,1.,0.));
#1967=DIRECTION('ref_axis',(-1.,0.,0.));
#1968=DIRECTION('',(1.,0.,0.));
#1969=DIRECTION('',(0.,0.,1.));
#1970=DIRECTION('',(-1.,0.,0.));
#1971=DIRECTION('',(0.,0.,-1.));
#1972=DIRECTION('center_axis',(0.,1.,0.));
#1973=DIRECTION('ref_axis',(-1.,0.,0.));
#1974=DIRECTION('',(1.,0.,0.));
#1975=DIRECTION('',(0.,0.,1.));
#1976=DIRECTION('',(-1.,0.,0.));
#1977=DIRECTION('',(0.,0.,-1.));
#1978=DIRECTION('center_axis',(0.,-1.,0.));
#1979=DIRECTION('ref_axis',(1.,0.,0.));
#1980=DIRECTION('',(-1.,0.,0.));
#1981=DIRECTION('',(0.,0.,1.));
#1982=DIRECTION('',(1.,0.,0.));
#1983=DIRECTION('',(0.,0.,1.));
#1984=DIRECTION('center_axis',(0.,-1.,0.));
#1985=DIRECTION('ref_axis',(1.,0.,0.));
#1986=DIRECTION('',(-1.,0.,0.));
#1987=DIRECTION('',(0.,0.,1.));
#1988=DIRECTION('',(1.,0.,0.));
#1989=DIRECTION('',(0.,0.,1.));
#1990=DIRECTION('center_axis',(0.,-1.,0.));
#1991=DIRECTION('ref_axis',(1.,0.,0.));
#1992=DIRECTION('',(-1.,0.,0.));
#1993=DIRECTION('',(0.,0.,1.));
#1994=DIRECTION('',(1.,0.,0.));
#1995=DIRECTION('',(0.,0.,1.));
#1996=DIRECTION('center_axis',(0.,-1.,0.));
#1997=DIRECTION('ref_axis',(1.,0.,0.));
#1998=DIRECTION('',(-1.,0.,0.));
#1999=DIRECTION('',(0.,0.,1.));
#2000=DIRECTION('',(1.,0.,0.));
#2001=DIRECTION('',(0.,0.,1.));
#2002=DIRECTION('center_axis',(0.,-1.,0.));
#2003=DIRECTION('ref_axis',(1.,0.,0.));
#2004=DIRECTION('',(-1.,0.,0.));
#2005=DIRECTION('',(0.,0.,1.));
#2006=DIRECTION('',(1.,0.,0.));
#2007=DIRECTION('',(0.,0.,1.));
#2008=DIRECTION('center_axis',(0.,-1.,0.));
#2009=DIRECTION('ref_axis',(1.,0.,0.));
#2010=DIRECTION('',(-1.,0.,0.));
#2011=DIRECTION('',(0.,0.,1.));
#2012=DIRECTION('',(1.,0.,0.));
#2013=DIRECTION('',(0.,0.,1.));
#2014=DIRECTION('center_axis',(-1.,0.,0.));
#2015=DIRECTION('ref_axis',(0.,-1.,0.));
#2016=DIRECTION('',(0.,-1.,0.));
#2017=DIRECTION('',(0.,0.,-1.));
#2018=DIRECTION('',(0.,1.,0.));
#2019=DIRECTION('',(0.,0.,1.));
#2020=DIRECTION('',(0.,-1.,0.));
#2021=DIRECTION('',(0.,-1.,0.));
#2022=DIRECTION('',(0.,0.,1.));
#2023=DIRECTION('',(0.,-1.,0.));
#2024=DIRECTION('',(0.,-1.,0.));
#2025=DIRECTION('',(0.,0.,1.));
#2026=DIRECTION('',(0.,-1.,0.));
#2027=DIRECTION('',(0.,-1.,0.));
#2028=DIRECTION('',(0.,0.,1.));
#2029=DIRECTION('',(0.,-1.,0.));
#2030=DIRECTION('',(0.,-1.,0.));
#2031=DIRECTION('',(0.,0.,1.));
#2032=DIRECTION('',(0.,-1.,0.));
#2033=DIRECTION('',(0.,-1.,0.));
#2034=DIRECTION('',(0.,0.,1.));
#2035=DIRECTION('',(0.,-1.,0.));
#2036=DIRECTION('',(0.,-1.,0.));
#2037=DIRECTION('',(0.,0.,1.));
#2038=DIRECTION('',(0.,-1.,0.));
#2039=DIRECTION('',(0.,0.,-1.));
#2040=DIRECTION('',(0.,-1.,0.));
#2041=DIRECTION('',(0.,-1.,0.));
#2042=DIRECTION('',(0.,0.,-1.));
#2043=DIRECTION('',(0.,-1.,0.));
#2044=DIRECTION('',(0.,-1.,0.));
#2045=DIRECTION('',(0.,0.,-1.));
#2046=DIRECTION('',(0.,-1.,0.));
#2047=DIRECTION('',(0.,-1.,0.));
#2048=DIRECTION('',(0.,0.,-1.));
#2049=DIRECTION('',(0.,-1.,0.));
#2050=DIRECTION('',(0.,-1.,0.));
#2051=DIRECTION('',(0.,0.,-1.));
#2052=DIRECTION('',(0.,-1.,0.));
#2053=DIRECTION('',(0.,-1.,0.));
#2054=DIRECTION('',(0.,0.,-1.));
#2055=DIRECTION('',(0.,-1.,0.));
#2056=DIRECTION('center_axis',(0.,0.,1.));
#2057=DIRECTION('ref_axis',(1.,0.,0.));
#2058=DIRECTION('',(-1.,0.,0.));
#2059=DIRECTION('',(0.,-1.,0.));
#2060=DIRECTION('center_axis',(0.,0.,1.));
#2061=DIRECTION('ref_axis',(1.,0.,0.));
#2062=DIRECTION('',(0.,-1.,0.));
#2063=DIRECTION('',(1.,0.,0.));
#2064=DIRECTION('center_axis',(1.,0.,0.));
#2065=DIRECTION('ref_axis',(0.,1.,0.));
#2066=DIRECTION('',(0.,0.,1.));
#2067=DIRECTION('',(0.,1.,0.));
#2068=DIRECTION('center_axis',(1.,0.,0.));
#2069=DIRECTION('ref_axis',(0.,1.,0.));
#2070=DIRECTION('',(0.,1.,0.));
#2071=DIRECTION('',(0.,0.,1.));
#2072=DIRECTION('center_axis',(0.,0.,1.));
#2073=DIRECTION('ref_axis',(1.,0.,0.));
#2074=DIRECTION('',(1.,0.,0.));
#2075=DIRECTION('center_axis',(0.,0.,1.));
#2076=DIRECTION('ref_axis',(1.,0.,0.));
#2077=DIRECTION('',(-1.,0.,0.));
#2078=DIRECTION('center_axis',(0.,0.,1.));
#2079=DIRECTION('ref_axis',(1.,0.,0.));
#2080=DIRECTION('',(-1.,0.,0.));
#2081=DIRECTION('',(0.,-1.,0.));
#2082=DIRECTION('center_axis',(0.,0.,1.));
#2083=DIRECTION('ref_axis',(1.,0.,0.));
#2084=DIRECTION('',(0.,-1.,0.));
#2085=DIRECTION('',(1.,0.,0.));
#2086=DIRECTION('center_axis',(1.,0.,0.));
#2087=DIRECTION('ref_axis',(0.,1.,0.));
#2088=DIRECTION('',(0.,0.,1.));
#2089=DIRECTION('',(0.,1.,0.));
#2090=DIRECTION('center_axis',(1.,0.,0.));
#2091=DIRECTION('ref_axis',(0.,1.,0.));
#2092=DIRECTION('',(0.,1.,0.));
#2093=DIRECTION('',(0.,0.,1.));
#2094=DIRECTION('center_axis',(0.,0.,1.));
#2095=DIRECTION('ref_axis',(1.,0.,0.));
#2096=DIRECTION('',(1.,0.,0.));
#2097=DIRECTION('center_axis',(0.,0.,1.));
#2098=DIRECTION('ref_axis',(1.,0.,0.));
#2099=DIRECTION('',(-1.,0.,0.));
#2100=DIRECTION('center_axis',(0.,0.,1.));
#2101=DIRECTION('ref_axis',(1.,0.,0.));
#2102=DIRECTION('',(-1.,0.,0.));
#2103=DIRECTION('',(0.,-1.,0.));
#2104=DIRECTION('center_axis',(0.,0.,1.));
#2105=DIRECTION('ref_axis',(1.,0.,0.));
#2106=DIRECTION('',(0.,-1.,0.));
#2107=DIRECTION('',(1.,0.,0.));
#2108=DIRECTION('center_axis',(1.,0.,0.));
#2109=DIRECTION('ref_axis',(0.,1.,0.));
#2110=DIRECTION('',(0.,0.,1.));
#2111=DIRECTION('',(0.,1.,0.));
#2112=DIRECTION('center_axis',(1.,0.,0.));
#2113=DIRECTION('ref_axis',(0.,1.,0.));
#2114=DIRECTION('',(0.,1.,0.));
#2115=DIRECTION('',(0.,0.,1.));
#2116=DIRECTION('center_axis',(0.,0.,1.));
#2117=DIRECTION('ref_axis',(1.,0.,0.));
#2118=DIRECTION('',(1.,0.,0.));
#2119=DIRECTION('center_axis',(0.,0.,1.));
#2120=DIRECTION('ref_axis',(1.,0.,0.));
#2121=DIRECTION('',(-1.,0.,0.));
#2122=DIRECTION('center_axis',(0.,0.,1.));
#2123=DIRECTION('ref_axis',(1.,0.,0.));
#2124=DIRECTION('',(-1.,0.,0.));
#2125=DIRECTION('',(0.,-1.,0.));
#2126=DIRECTION('center_axis',(0.,0.,1.));
#2127=DIRECTION('ref_axis',(1.,0.,0.));
#2128=DIRECTION('',(0.,-1.,0.));
#2129=DIRECTION('',(1.,0.,0.));
#2130=DIRECTION('center_axis',(1.,0.,0.));
#2131=DIRECTION('ref_axis',(0.,1.,0.));
#2132=DIRECTION('',(0.,0.,1.));
#2133=DIRECTION('',(0.,1.,0.));
#2134=DIRECTION('center_axis',(1.,0.,0.));
#2135=DIRECTION('ref_axis',(0.,1.,0.));
#2136=DIRECTION('',(0.,1.,0.));
#2137=DIRECTION('',(0.,0.,1.));
#2138=DIRECTION('center_axis',(0.,0.,1.));
#2139=DIRECTION('ref_axis',(1.,0.,0.));
#2140=DIRECTION('',(1.,0.,0.));
#2141=DIRECTION('center_axis',(0.,0.,1.));
#2142=DIRECTION('ref_axis',(1.,0.,0.));
#2143=DIRECTION('',(-1.,0.,0.));
#2144=DIRECTION('center_axis',(0.,0.,1.));
#2145=DIRECTION('ref_axis',(1.,0.,0.));
#2146=DIRECTION('',(-1.,0.,0.));
#2147=DIRECTION('',(0.,-1.,0.));
#2148=DIRECTION('center_axis',(0.,0.,1.));
#2149=DIRECTION('ref_axis',(1.,0.,0.));
#2150=DIRECTION('',(0.,-1.,0.));
#2151=DIRECTION('',(1.,0.,0.));
#2152=DIRECTION('center_axis',(1.,0.,0.));
#2153=DIRECTION('ref_axis',(0.,1.,0.));
#2154=DIRECTION('',(0.,0.,1.));
#2155=DIRECTION('',(0.,1.,0.));
#2156=DIRECTION('center_axis',(1.,0.,0.));
#2157=DIRECTION('ref_axis',(0.,1.,0.));
#2158=DIRECTION('',(0.,1.,0.));
#2159=DIRECTION('',(0.,0.,1.));
#2160=DIRECTION('center_axis',(0.,0.,1.));
#2161=DIRECTION('ref_axis',(1.,0.,0.));
#2162=DIRECTION('',(1.,0.,0.));
#2163=DIRECTION('center_axis',(0.,0.,1.));
#2164=DIRECTION('ref_axis',(1.,0.,0.));
#2165=DIRECTION('',(-1.,0.,0.));
#2166=DIRECTION('center_axis',(0.,0.,1.));
#2167=DIRECTION('ref_axis',(1.,0.,0.));
#2168=DIRECTION('',(-1.,0.,0.));
#2169=DIRECTION('',(0.,-1.,0.));
#2170=DIRECTION('center_axis',(0.,0.,1.));
#2171=DIRECTION('ref_axis',(1.,0.,0.));
#2172=DIRECTION('',(0.,-1.,0.));
#2173=DIRECTION('',(1.,0.,0.));
#2174=DIRECTION('center_axis',(1.,0.,0.));
#2175=DIRECTION('ref_axis',(0.,1.,0.));
#2176=DIRECTION('',(0.,0.,1.));
#2177=DIRECTION('',(0.,1.,0.));
#2178=DIRECTION('center_axis',(1.,0.,0.));
#2179=DIRECTION('ref_axis',(0.,1.,0.));
#2180=DIRECTION('',(0.,1.,0.));
#2181=DIRECTION('',(0.,0.,1.));
#2182=DIRECTION('center_axis',(0.,0.,1.));
#2183=DIRECTION('ref_axis',(1.,0.,0.));
#2184=DIRECTION('',(1.,0.,0.));
#2185=DIRECTION('center_axis',(0.,0.,1.));
#2186=DIRECTION('ref_axis',(1.,0.,0.));
#2187=DIRECTION('',(-1.,0.,0.));
#2188=DIRECTION('center_axis',(0.,1.,0.));
#2189=DIRECTION('ref_axis',(-1.,0.,0.));
#2190=DIRECTION('',(-1.,0.,0.));
#2191=DIRECTION('',(0.,0.,1.));
#2192=DIRECTION('',(-1.,0.,0.));
#2193=DIRECTION('center_axis',(0.,0.,1.));
#2194=DIRECTION('ref_axis',(1.,0.,0.));
#2195=DIRECTION('',(1.,0.,0.));
#2196=DIRECTION('',(0.,-1.,0.));
#2197=DIRECTION('center_axis',(0.,-1.,0.));
#2198=DIRECTION('ref_axis',(1.,0.,0.));
#2199=DIRECTION('',(1.,0.,0.));
#2200=DIRECTION('',(0.,0.,1.));
#2201=DIRECTION('center_axis',(-1.,0.,0.));
#2202=DIRECTION('ref_axis',(0.,-1.,0.));
#2203=DIRECTION('',(0.,-1.,0.));
#2204=DIRECTION('center_axis',(0.,0.,1.));
#2205=DIRECTION('ref_axis',(1.,0.,0.));
#2206=DIRECTION('axis',(0.,0.,1.));
#2207=DIRECTION('refdir',(1.,0.,0.));
#2208=DIRECTION('center_axis',(0.,-1.,0.));
#2209=DIRECTION('ref_axis',(1.,0.,0.));
#2210=DIRECTION('',(-1.,0.,0.));
#2211=DIRECTION('',(0.,0.,1.));
#2212=DIRECTION('',(1.,0.,0.));
#2213=DIRECTION('',(0.,0.,-1.));
#2214=DIRECTION('center_axis',(0.,1.,0.));
#2215=DIRECTION('ref_axis',(-1.,0.,0.));
#2216=DIRECTION('',(1.,0.,0.));
#2217=DIRECTION('',(0.,0.,1.));
#2218=DIRECTION('',(-1.,0.,0.));
#2219=DIRECTION('',(0.,0.,-1.));
#2220=DIRECTION('center_axis',(0.,0.,1.));
#2221=DIRECTION('ref_axis',(1.,0.,0.));
#2222=DIRECTION('',(0.,1.,0.));
#2223=DIRECTION('',(0.,-1.,0.));
#2224=DIRECTION('center_axis',(1.,0.,0.));
#2225=DIRECTION('ref_axis',(0.,1.,0.));
#2226=DIRECTION('',(0.,1.,0.));
#2227=DIRECTION('',(0.,0.,1.));
#2228=DIRECTION('',(0.,1.,0.));
#2229=DIRECTION('',(0.,0.,1.));
#2230=DIRECTION('',(0.,1.,0.));
#2231=DIRECTION('center_axis',(0.,0.,1.));
#2232=DIRECTION('ref_axis',(1.,0.,0.));
#2233=DIRECTION('',(0.,-1.,0.));
#2234=DIRECTION('',(1.,0.,0.));
#2235=DIRECTION('center_axis',(0.,1.,0.));
#2236=DIRECTION('ref_axis',(-1.,0.,0.));
#2237=DIRECTION('',(-1.,0.,0.));
#2238=DIRECTION('',(0.,0.,1.));
#2239=DIRECTION('',(-1.,0.,0.));
#2240=DIRECTION('center_axis',(0.,-1.,0.));
#2241=DIRECTION('ref_axis',(1.,0.,0.));
#2242=DIRECTION('',(1.,0.,0.));
#2243=DIRECTION('',(0.,0.,1.));
#2244=DIRECTION('center_axis',(-1.,0.,0.));
#2245=DIRECTION('ref_axis',(0.,-1.,0.));
#2246=DIRECTION('',(0.,-1.,0.));
#2247=DIRECTION('',(0.,-1.,0.));
#2248=DIRECTION('center_axis',(0.,0.,1.));
#2249=DIRECTION('ref_axis',(1.,0.,0.));
#2250=DIRECTION('center_axis',(0.,0.,1.));
#2251=DIRECTION('ref_axis',(1.,0.,0.));
#2252=DIRECTION('axis',(0.,0.,1.));
#2253=DIRECTION('refdir',(1.,0.,0.));
#2254=DIRECTION('center_axis',(0.,1.,0.));
#2255=DIRECTION('ref_axis',(-1.,0.,0.));
#2256=DIRECTION('',(-1.,0.,0.));
#2257=DIRECTION('',(0.,0.,1.));
#2258=DIRECTION('',(-1.,0.,0.));
#2259=DIRECTION('',(0.,0.,1.));
#2260=DIRECTION('center_axis',(1.,0.,0.));
#2261=DIRECTION('ref_axis',(0.,1.,0.));
#2262=DIRECTION('',(0.,1.,0.));
#2263=DIRECTION('',(0.,1.,0.));
#2264=DIRECTION('',(0.,0.,1.));
#2265=DIRECTION('center_axis',(0.,-1.,0.));
#2266=DIRECTION('ref_axis',(1.,0.,0.));
#2267=DIRECTION('',(1.,0.,0.));
#2268=DIRECTION('',(1.,0.,0.));
#2269=DIRECTION('',(0.,0.,1.));
#2270=DIRECTION('center_axis',(-1.,0.,0.));
#2271=DIRECTION('ref_axis',(0.,-1.,0.));
#2272=DIRECTION('',(0.,-1.,0.));
#2273=DIRECTION('',(0.,-1.,0.));
#2274=DIRECTION('center_axis',(0.,0.,1.));
#2275=DIRECTION('ref_axis',(1.,0.,0.));
#2276=DIRECTION('center_axis',(0.,0.,1.));
#2277=DIRECTION('ref_axis',(1.,0.,0.));
#2278=DIRECTION('axis',(0.,0.,1.));
#2279=DIRECTION('refdir',(1.,0.,0.));
#2280=DIRECTION('center_axis',(0.,1.,0.));
#2281=DIRECTION('ref_axis',(-1.,0.,0.));
#2282=DIRECTION('',(-1.,0.,0.));
#2283=DIRECTION('',(0.,0.,1.));
#2284=DIRECTION('',(-1.,0.,0.));
#2285=DIRECTION('',(0.,0.,1.));
#2286=DIRECTION('center_axis',(1.,0.,0.));
#2287=DIRECTION('ref_axis',(0.,1.,0.));
#2288=DIRECTION('',(0.,1.,0.));
#2289=DIRECTION('',(0.,1.,0.));
#2290=DIRECTION('',(0.,0.,1.));
#2291=DIRECTION('center_axis',(0.,-1.,0.));
#2292=DIRECTION('ref_axis',(1.,0.,0.));
#2293=DIRECTION('',(1.,0.,0.));
#2294=DIRECTION('',(1.,0.,0.));
#2295=DIRECTION('',(0.,0.,1.));
#2296=DIRECTION('center_axis',(-1.,0.,0.));
#2297=DIRECTION('ref_axis',(0.,-1.,0.));
#2298=DIRECTION('',(0.,-1.,0.));
#2299=DIRECTION('',(0.,-1.,0.));
#2300=DIRECTION('center_axis',(0.,0.,1.));
#2301=DIRECTION('ref_axis',(1.,0.,0.));
#2302=DIRECTION('center_axis',(0.,0.,1.));
#2303=DIRECTION('ref_axis',(1.,0.,0.));
#2304=DIRECTION('axis',(0.,0.,1.));
#2305=DIRECTION('refdir',(1.,0.,0.));
#2306=DIRECTION('center_axis',(0.,0.,1.));
#2307=DIRECTION('ref_axis',(1.,0.,0.));
#2308=DIRECTION('center_axis',(0.,0.,1.));
#2309=DIRECTION('ref_axis',(1.,0.,0.));
#2310=DIRECTION('',(0.,0.,-1.));
#2311=DIRECTION('center_axis',(0.,0.,1.));
#2312=DIRECTION('ref_axis',(1.,0.,0.));
#2313=DIRECTION('center_axis',(0.,0.,1.));
#2314=DIRECTION('ref_axis',(1.,0.,0.));
#2315=DIRECTION('center_axis',(0.,0.,1.));
#2316=DIRECTION('ref_axis',(1.,0.,0.));
#2317=DIRECTION('',(0.,0.,1.));
#2318=DIRECTION('',(1.,0.,0.));
#2319=DIRECTION('',(0.,0.,1.));
#2320=DIRECTION('',(1.,0.,0.));
#2321=DIRECTION('',(0.,0.,1.));
#2322=DIRECTION('',(1.,0.,0.));
#2323=DIRECTION('',(0.,0.,1.));
#2324=DIRECTION('',(1.,0.,0.));
#2325=DIRECTION('',(1.,0.,2.22044604925031E-16));
#2326=DIRECTION('',(2.22044604925031E-16,0.,-1.));
#2327=DIRECTION('',(1.22464679914735E-16,0.,-1.));
#2328=DIRECTION('',(-1.,0.,-1.22464679914735E-16));
#2329=DIRECTION('',(1.22464679914735E-16,0.,-1.));
#2330=DIRECTION('',(-1.,0.,-1.22464679914735E-16));
#2331=DIRECTION('',(0.,0.,1.));
#2332=DIRECTION('',(1.,0.,0.));
#2333=DIRECTION('',(0.,0.,1.));
#2334=DIRECTION('',(1.,0.,0.));
#2335=DIRECTION('',(0.,0.,1.));
#2336=DIRECTION('',(1.,0.,0.));
#2337=DIRECTION('',(0.,0.,1.));
#2338=DIRECTION('',(1.,0.,0.));
#2339=DIRECTION('',(0.,0.,1.));
#2340=DIRECTION('',(1.,0.,0.));
#2341=DIRECTION('',(1.22464679914735E-16,0.,-1.));
#2342=DIRECTION('',(-1.,0.,-1.22464679914735E-16));
#2343=DIRECTION('',(0.,0.,1.));
#2344=DIRECTION('',(1.,0.,0.));
#2345=DIRECTION('',(1.22464679914735E-16,0.,-1.));
#2346=DIRECTION('',(-1.,0.,-1.22464679914735E-16));
#2347=DIRECTION('',(0.,0.,1.));
#2348=DIRECTION('',(1.,0.,0.));
#2349=DIRECTION('',(0.,0.,1.));
#2350=DIRECTION('',(1.,0.,0.));
#2351=DIRECTION('',(0.,0.,1.));
#2352=DIRECTION('',(1.,0.,0.));
#2353=DIRECTION('',(0.,0.,1.));
#2354=DIRECTION('',(1.,0.,0.));
#2355=DIRECTION('',(0.,0.,1.));
#2356=DIRECTION('',(1.,0.,0.));
#2357=DIRECTION('',(0.,0.,1.));
#2358=DIRECTION('',(1.,0.,0.));
#2359=DIRECTION('',(1.,0.,2.22044604925031E-16));
#2360=DIRECTION('',(2.22044604925031E-16,0.,-1.));
#2361=DIRECTION('',(1.,0.,2.22044604925031E-16));
#2362=DIRECTION('',(2.22044604925031E-16,0.,-1.));
#2363=DIRECTION('',(1.,0.,2.22044604925031E-16));
#2364=DIRECTION('',(2.22044604925031E-16,0.,-1.));
#2365=CARTESIAN_POINT('',(0.,0.,0.));
#2366=CARTESIAN_POINT('',(0.,0.,0.));
#2367=CARTESIAN_POINT('Origin',(0.,51.,64.));
#2368=CARTESIAN_POINT('',(0.,51.,64.41));
#2369=CARTESIAN_POINT('Origin',(0.,51.,64.));
#2370=CARTESIAN_POINT('',(1.5,51.,64.41));
#2371=CARTESIAN_POINT('',(0.,51.,64.41));
#2372=CARTESIAN_POINT('Origin',(1.5,51.,64.));
#2373=CARTESIAN_POINT('Origin',(1.5,51.,64.));
#2374=CARTESIAN_POINT('Origin',(0.,9.,116.));
#2375=CARTESIAN_POINT('',(0.,9.,116.41));
#2376=CARTESIAN_POINT('Origin',(0.,9.,116.));
#2377=CARTESIAN_POINT('',(1.5,9.,116.41));
#2378=CARTESIAN_POINT('',(0.,9.,116.41));
#2379=CARTESIAN_POINT('Origin',(1.5,9.,116.));
#2380=CARTESIAN_POINT('Origin',(1.5,9.,116.));
#2381=CARTESIAN_POINT('Origin',(0.,9.,64.));
#2382=CARTESIAN_POINT('',(0.,9.,64.41));
#2383=CARTESIAN_POINT('Origin',(0.,9.,64.));
#2384=CARTESIAN_POINT('',(1.5,9.,64.41));
#2385=CARTESIAN_POINT('',(0.,9.,64.41));
#2386=CARTESIAN_POINT('Origin',(1.5,9.,64.));
#2387=CARTESIAN_POINT('Origin',(1.5,9.,64.));
#2388=CARTESIAN_POINT('Origin',(0.,51.,116.));
#2389=CARTESIAN_POINT('',(0.,51.,116.41));
#2390=CARTESIAN_POINT('Origin',(0.,51.,116.));
#2391=CARTESIAN_POINT('',(1.5,51.,116.41));
#2392=CARTESIAN_POINT('',(0.,51.,116.41));
#2393=CARTESIAN_POINT('Origin',(1.5,51.,116.));
#2394=CARTESIAN_POINT('Origin',(1.5,51.,116.));
#2395=CARTESIAN_POINT('Origin',(1.81,58.82,0.));
#2396=CARTESIAN_POINT('',(1.3,58.82,149.08));
#2397=CARTESIAN_POINT('',(1.8,58.82,149.08));
#2398=CARTESIAN_POINT('',(1.6825,58.82,149.08));
#2399=CARTESIAN_POINT('',(1.3,58.82,120.92));
#2400=CARTESIAN_POINT('',(1.3,58.82,0.));
#2401=CARTESIAN_POINT('',(1.8,58.82,120.92));
#2402=CARTESIAN_POINT('',(1.6825,58.82,120.92));
#2403=CARTESIAN_POINT('',(1.8,58.82,0.));
#2404=CARTESIAN_POINT('Origin',(1.81,58.82,0.));
#2405=CARTESIAN_POINT('',(1.3,58.82,119.08));
#2406=CARTESIAN_POINT('',(1.8,58.82,119.08));
#2407=CARTESIAN_POINT('',(1.6825,58.82,119.08));
#2408=CARTESIAN_POINT('',(1.3,58.82,90.92));
#2409=CARTESIAN_POINT('',(1.3,58.82,0.));
#2410=CARTESIAN_POINT('',(1.8,58.82,90.92));
#2411=CARTESIAN_POINT('',(1.6825,58.82,90.92));
#2412=CARTESIAN_POINT('',(1.8,58.82,0.));
#2413=CARTESIAN_POINT('Origin',(1.81,58.82,0.));
#2414=CARTESIAN_POINT('',(1.3,58.82,89.08));
#2415=CARTESIAN_POINT('',(1.8,58.82,89.08));
#2416=CARTESIAN_POINT('',(1.6825,58.82,89.08));
#2417=CARTESIAN_POINT('',(1.3,58.82,60.92));
#2418=CARTESIAN_POINT('',(1.3,58.82,0.));
#2419=CARTESIAN_POINT('',(1.8,58.82,60.92));
#2420=CARTESIAN_POINT('',(1.6825,58.82,60.92));
#2421=CARTESIAN_POINT('',(1.8,58.82,0.));
#2422=CARTESIAN_POINT('Origin',(1.81,58.82,0.));
#2423=CARTESIAN_POINT('',(1.3,58.82,59.08));
#2424=CARTESIAN_POINT('',(1.8,58.82,59.08));
#2425=CARTESIAN_POINT('',(1.6825,58.82,59.08));
#2426=CARTESIAN_POINT('',(1.3,58.82,30.92));
#2427=CARTESIAN_POINT('',(1.3,58.82,0.));
#2428=CARTESIAN_POINT('',(1.8,58.82,30.92));
#2429=CARTESIAN_POINT('',(1.6825,58.82,30.92));
#2430=CARTESIAN_POINT('',(1.8,58.82,0.));
#2431=CARTESIAN_POINT('Origin',(1.81,58.82,0.));
#2432=CARTESIAN_POINT('',(1.3,58.82,29.08));
#2433=CARTESIAN_POINT('',(1.8,58.82,29.08));
#2434=CARTESIAN_POINT('',(1.6825,58.82,29.08));
#2435=CARTESIAN_POINT('',(1.3,58.82,1.82));
#2436=CARTESIAN_POINT('',(1.3,58.82,0.));
#2437=CARTESIAN_POINT('',(1.8,58.82,1.82));
#2438=CARTESIAN_POINT('',(1.6825,58.82,1.82));
#2439=CARTESIAN_POINT('',(1.8,58.82,0.));
#2440=CARTESIAN_POINT('Origin',(1.81,58.82,0.));
#2441=CARTESIAN_POINT('',(1.3,58.82,178.18));
#2442=CARTESIAN_POINT('',(1.8,58.82,178.18));
#2443=CARTESIAN_POINT('',(1.6825,58.82,178.18));
#2444=CARTESIAN_POINT('',(1.3,58.82,150.92));
#2445=CARTESIAN_POINT('',(1.3,58.82,0.));
#2446=CARTESIAN_POINT('',(1.8,58.82,150.92));
#2447=CARTESIAN_POINT('',(1.6825,58.82,150.92));
#2448=CARTESIAN_POINT('',(1.8,58.82,0.));
#2449=CARTESIAN_POINT('Origin',(1.3,58.18,0.));
#2450=CARTESIAN_POINT('',(1.8,58.18,29.08));
#2451=CARTESIAN_POINT('',(1.3,58.18,29.08));
#2452=CARTESIAN_POINT('',(1.4275,58.18,29.08));
#2453=CARTESIAN_POINT('',(1.8,58.18,1.82));
#2454=CARTESIAN_POINT('',(1.8,58.18,0.));
#2455=CARTESIAN_POINT('',(1.3,58.18,1.82));
#2456=CARTESIAN_POINT('',(1.4275,58.18,1.82));
#2457=CARTESIAN_POINT('',(1.3,58.18,0.));
#2458=CARTESIAN_POINT('Origin',(1.3,58.18,0.));
#2459=CARTESIAN_POINT('',(1.8,58.18,59.08));
#2460=CARTESIAN_POINT('',(1.3,58.18,59.08));
#2461=CARTESIAN_POINT('',(1.4275,58.18,59.08));
#2462=CARTESIAN_POINT('',(1.8,58.18,30.92));
#2463=CARTESIAN_POINT('',(1.8,58.18,0.));
#2464=CARTESIAN_POINT('',(1.3,58.18,30.92));
#2465=CARTESIAN_POINT('',(1.4275,58.18,30.92));
#2466=CARTESIAN_POINT('',(1.3,58.18,0.));
#2467=CARTESIAN_POINT('Origin',(1.3,58.18,0.));
#2468=CARTESIAN_POINT('',(1.8,58.18,89.08));
#2469=CARTESIAN_POINT('',(1.3,58.18,89.08));
#2470=CARTESIAN_POINT('',(1.4275,58.18,89.08));
#2471=CARTESIAN_POINT('',(1.8,58.18,60.92));
#2472=CARTESIAN_POINT('',(1.8,58.18,0.));
#2473=CARTESIAN_POINT('',(1.3,58.18,60.92));
#2474=CARTESIAN_POINT('',(1.4275,58.18,60.92));
#2475=CARTESIAN_POINT('',(1.3,58.18,0.));
#2476=CARTESIAN_POINT('Origin',(1.3,58.18,0.));
#2477=CARTESIAN_POINT('',(1.8,58.18,119.08));
#2478=CARTESIAN_POINT('',(1.3,58.18,119.08));
#2479=CARTESIAN_POINT('',(1.4275,58.18,119.08));
#2480=CARTESIAN_POINT('',(1.8,58.18,90.92));
#2481=CARTESIAN_POINT('',(1.8,58.18,0.));
#2482=CARTESIAN_POINT('',(1.3,58.18,90.92));
#2483=CARTESIAN_POINT('',(1.4275,58.18,90.92));
#2484=CARTESIAN_POINT('',(1.3,58.18,0.));
#2485=CARTESIAN_POINT('Origin',(1.3,58.18,0.));
#2486=CARTESIAN_POINT('',(1.8,58.18,149.08));
#2487=CARTESIAN_POINT('',(1.3,58.18,149.08));
#2488=CARTESIAN_POINT('',(1.4275,58.18,149.08));
#2489=CARTESIAN_POINT('',(1.8,58.18,120.92));
#2490=CARTESIAN_POINT('',(1.8,58.18,0.));
#2491=CARTESIAN_POINT('',(1.3,58.18,120.92));
#2492=CARTESIAN_POINT('',(1.4275,58.18,120.92));
#2493=CARTESIAN_POINT('',(1.3,58.18,0.));
#2494=CARTESIAN_POINT('Origin',(1.3,58.18,0.));
#2495=CARTESIAN_POINT('',(1.8,58.18,178.18));
#2496=CARTESIAN_POINT('',(1.3,58.18,178.18));
#2497=CARTESIAN_POINT('',(1.4275,58.18,178.18));
#2498=CARTESIAN_POINT('',(1.8,58.18,150.92));
#2499=CARTESIAN_POINT('',(1.8,58.18,0.));
#2500=CARTESIAN_POINT('',(1.3,58.18,150.92));
#2501=CARTESIAN_POINT('',(1.4275,58.18,150.92));
#2502=CARTESIAN_POINT('',(1.3,58.18,0.));
#2503=CARTESIAN_POINT('Origin',(1.3,60.,178.18));
#2504=CARTESIAN_POINT('',(1.3,60.,178.18));
#2505=CARTESIAN_POINT('',(1.3,60.,178.18));
#2506=CARTESIAN_POINT('',(1.3,60.,180.));
#2507=CARTESIAN_POINT('',(1.3,60.,89.09));
#2508=CARTESIAN_POINT('',(1.3,0.,180.));
#2509=CARTESIAN_POINT('',(1.3,45.,180.));
#2510=CARTESIAN_POINT('',(1.3,0.,178.18));
#2511=CARTESIAN_POINT('',(1.3,0.,89.09));
#2512=CARTESIAN_POINT('',(1.3,60.,178.18));
#2513=CARTESIAN_POINT('',(1.3,0.,150.92));
#2514=CARTESIAN_POINT('',(1.3,60.,150.92));
#2515=CARTESIAN_POINT('',(1.3,0.,149.08));
#2516=CARTESIAN_POINT('',(1.3,0.,74.54));
#2517=CARTESIAN_POINT('',(1.3,60.,149.08));
#2518=CARTESIAN_POINT('',(1.3,0.,120.92));
#2519=CARTESIAN_POINT('',(1.3,60.,120.92));
#2520=CARTESIAN_POINT('',(1.3,0.,119.08));
#2521=CARTESIAN_POINT('',(1.3,0.,59.54));
#2522=CARTESIAN_POINT('',(1.3,60.,119.08));
#2523=CARTESIAN_POINT('',(1.3,0.,90.92));
#2524=CARTESIAN_POINT('',(1.3,60.,90.92));
#2525=CARTESIAN_POINT('',(1.3,0.,89.08));
#2526=CARTESIAN_POINT('',(1.3,0.,44.54));
#2527=CARTESIAN_POINT('',(1.3,60.,89.08));
#2528=CARTESIAN_POINT('',(1.3,0.,60.92));
#2529=CARTESIAN_POINT('',(1.3,60.,60.92));
#2530=CARTESIAN_POINT('',(1.3,0.,59.08));
#2531=CARTESIAN_POINT('',(1.3,0.,29.54));
#2532=CARTESIAN_POINT('',(1.3,60.,59.08));
#2533=CARTESIAN_POINT('',(1.3,0.,30.92));
#2534=CARTESIAN_POINT('',(1.3,60.,30.92));
#2535=CARTESIAN_POINT('',(1.3,0.,29.08));
#2536=CARTESIAN_POINT('',(1.3,0.,14.54));
#2537=CARTESIAN_POINT('',(1.3,60.,29.08));
#2538=CARTESIAN_POINT('',(1.3,0.,1.82));
#2539=CARTESIAN_POINT('',(1.3,60.,1.82));
#2540=CARTESIAN_POINT('',(1.3,0.,0.));
#2541=CARTESIAN_POINT('',(1.3,0.,0.));
#2542=CARTESIAN_POINT('',(1.3,60.,0.));
#2543=CARTESIAN_POINT('',(1.3,45.,0.));
#2544=CARTESIAN_POINT('',(1.3,60.,1.82));
#2545=CARTESIAN_POINT('',(1.3,60.,0.));
#2546=CARTESIAN_POINT('',(1.3,60.,1.82));
#2547=CARTESIAN_POINT('',(1.3,60.,29.08));
#2548=CARTESIAN_POINT('',(1.3,60.,29.08));
#2549=CARTESIAN_POINT('',(1.3,60.,30.92));
#2550=CARTESIAN_POINT('',(1.3,60.,14.54));
#2551=CARTESIAN_POINT('',(1.3,60.,30.92));
#2552=CARTESIAN_POINT('',(1.3,60.,59.08));
#2553=CARTESIAN_POINT('',(1.3,60.,59.08));
#2554=CARTESIAN_POINT('',(1.3,60.,60.92));
#2555=CARTESIAN_POINT('',(1.3,60.,29.54));
#2556=CARTESIAN_POINT('',(1.3,60.,60.92));
#2557=CARTESIAN_POINT('',(1.3,60.,89.08));
#2558=CARTESIAN_POINT('',(1.3,60.,89.08));
#2559=CARTESIAN_POINT('',(1.3,60.,90.92));
#2560=CARTESIAN_POINT('',(1.3,60.,44.54));
#2561=CARTESIAN_POINT('',(1.3,60.,90.92));
#2562=CARTESIAN_POINT('',(1.3,60.,119.08));
#2563=CARTESIAN_POINT('',(1.3,60.,119.08));
#2564=CARTESIAN_POINT('',(1.3,60.,120.92));
#2565=CARTESIAN_POINT('',(1.3,60.,59.54));
#2566=CARTESIAN_POINT('',(1.3,60.,120.92));
#2567=CARTESIAN_POINT('',(1.3,60.,149.08));
#2568=CARTESIAN_POINT('',(1.3,60.,149.08));
#2569=CARTESIAN_POINT('',(1.3,60.,150.92));
#2570=CARTESIAN_POINT('',(1.3,60.,74.54));
#2571=CARTESIAN_POINT('',(1.3,60.,150.92));
#2572=CARTESIAN_POINT('Origin',(1.555,30.,178.18));
#2573=CARTESIAN_POINT('',(1.8,0.,178.18));
#2574=CARTESIAN_POINT('',(0.7775,0.,178.18));
#2575=CARTESIAN_POINT('',(1.8,15.,178.18));
#2576=CARTESIAN_POINT('Origin',(1.555,30.,178.18));
#2577=CARTESIAN_POINT('',(1.8,60.,178.18));
#2578=CARTESIAN_POINT('',(1.8,15.,178.18));
#2579=CARTESIAN_POINT('',(1.6775,60.,178.18));
#2580=CARTESIAN_POINT('Origin',(1.8,0.,0.));
#2581=CARTESIAN_POINT('',(1.8,0.,150.92));
#2582=CARTESIAN_POINT('',(1.8,0.,0.));
#2583=CARTESIAN_POINT('',(1.8,15.,150.92));
#2584=CARTESIAN_POINT('Origin',(1.8,0.,0.));
#2585=CARTESIAN_POINT('',(1.8,60.,150.92));
#2586=CARTESIAN_POINT('',(1.8,15.,150.92));
#2587=CARTESIAN_POINT('',(1.8,60.,0.));
#2588=CARTESIAN_POINT('Origin',(1.555,30.,150.92));
#2589=CARTESIAN_POINT('',(0.7775,0.,150.92));
#2590=CARTESIAN_POINT('Origin',(1.555,30.,150.92));
#2591=CARTESIAN_POINT('',(1.6775,60.,150.92));
#2592=CARTESIAN_POINT('Origin',(1.555,30.,149.08));
#2593=CARTESIAN_POINT('',(1.8,0.,149.08));
#2594=CARTESIAN_POINT('',(0.7775,0.,149.08));
#2595=CARTESIAN_POINT('',(1.8,15.,149.08));
#2596=CARTESIAN_POINT('Origin',(1.555,30.,149.08));
#2597=CARTESIAN_POINT('',(1.8,60.,149.08));
#2598=CARTESIAN_POINT('',(1.8,15.,149.08));
#2599=CARTESIAN_POINT('',(1.6775,60.,149.08));
#2600=CARTESIAN_POINT('Origin',(1.8,0.,0.));
#2601=CARTESIAN_POINT('',(1.8,0.,120.92));
#2602=CARTESIAN_POINT('',(1.8,0.,0.));
#2603=CARTESIAN_POINT('',(1.8,15.,120.92));
#2604=CARTESIAN_POINT('Origin',(1.8,0.,0.));
#2605=CARTESIAN_POINT('',(1.8,60.,120.92));
#2606=CARTESIAN_POINT('',(1.8,15.,120.92));
#2607=CARTESIAN_POINT('',(1.8,60.,0.));
#2608=CARTESIAN_POINT('Origin',(1.555,30.,120.92));
#2609=CARTESIAN_POINT('',(0.7775,0.,120.92));
#2610=CARTESIAN_POINT('Origin',(1.555,30.,120.92));
#2611=CARTESIAN_POINT('',(1.6775,60.,120.92));
#2612=CARTESIAN_POINT('Origin',(1.555,30.,119.08));
#2613=CARTESIAN_POINT('',(1.8,0.,119.08));
#2614=CARTESIAN_POINT('',(0.7775,0.,119.08));
#2615=CARTESIAN_POINT('',(1.8,15.,119.08));
#2616=CARTESIAN_POINT('Origin',(1.555,30.,119.08));
#2617=CARTESIAN_POINT('',(1.8,60.,119.08));
#2618=CARTESIAN_POINT('',(1.8,15.,119.08));
#2619=CARTESIAN_POINT('',(1.6775,60.,119.08));
#2620=CARTESIAN_POINT('Origin',(1.8,0.,0.));
#2621=CARTESIAN_POINT('',(1.8,0.,90.92));
#2622=CARTESIAN_POINT('',(1.8,0.,0.));
#2623=CARTESIAN_POINT('',(1.8,15.,90.92));
#2624=CARTESIAN_POINT('Origin',(1.8,0.,0.));
#2625=CARTESIAN_POINT('',(1.8,60.,90.92));
#2626=CARTESIAN_POINT('',(1.8,15.,90.92));
#2627=CARTESIAN_POINT('',(1.8,60.,0.));
#2628=CARTESIAN_POINT('Origin',(1.555,30.,90.92));
#2629=CARTESIAN_POINT('',(0.7775,0.,90.92));
#2630=CARTESIAN_POINT('Origin',(1.555,30.,90.92));
#2631=CARTESIAN_POINT('',(1.6775,60.,90.92));
#2632=CARTESIAN_POINT('Origin',(1.555,30.,89.08));
#2633=CARTESIAN_POINT('',(1.8,0.,89.08));
#2634=CARTESIAN_POINT('',(0.7775,0.,89.08));
#2635=CARTESIAN_POINT('',(1.8,15.,89.08));
#2636=CARTESIAN_POINT('Origin',(1.555,30.,89.08));
#2637=CARTESIAN_POINT('',(1.8,60.,89.08));
#2638=CARTESIAN_POINT('',(1.8,15.,89.08));
#2639=CARTESIAN_POINT('',(1.6775,60.,89.08));
#2640=CARTESIAN_POINT('Origin',(1.8,0.,0.));
#2641=CARTESIAN_POINT('',(1.8,0.,60.92));
#2642=CARTESIAN_POINT('',(1.8,0.,0.));
#2643=CARTESIAN_POINT('',(1.8,15.,60.92));
#2644=CARTESIAN_POINT('Origin',(1.8,0.,0.));
#2645=CARTESIAN_POINT('',(1.8,60.,60.92));
#2646=CARTESIAN_POINT('',(1.8,15.,60.92));
#2647=CARTESIAN_POINT('',(1.8,60.,0.));
#2648=CARTESIAN_POINT('Origin',(1.555,30.,60.92));
#2649=CARTESIAN_POINT('',(0.7775,0.,60.92));
#2650=CARTESIAN_POINT('Origin',(1.555,30.,60.92));
#2651=CARTESIAN_POINT('',(1.6775,60.,60.92));
#2652=CARTESIAN_POINT('Origin',(1.555,30.,59.08));
#2653=CARTESIAN_POINT('',(1.8,0.,59.08));
#2654=CARTESIAN_POINT('',(0.7775,0.,59.08));
#2655=CARTESIAN_POINT('',(1.8,15.,59.08));
#2656=CARTESIAN_POINT('Origin',(1.555,30.,59.08));
#2657=CARTESIAN_POINT('',(1.8,60.,59.08));
#2658=CARTESIAN_POINT('',(1.8,15.,59.08));
#2659=CARTESIAN_POINT('',(1.6775,60.,59.08));
#2660=CARTESIAN_POINT('Origin',(1.8,0.,0.));
#2661=CARTESIAN_POINT('',(1.8,0.,30.92));
#2662=CARTESIAN_POINT('',(1.8,0.,0.));
#2663=CARTESIAN_POINT('',(1.8,15.,30.92));
#2664=CARTESIAN_POINT('Origin',(1.8,0.,0.));
#2665=CARTESIAN_POINT('',(1.8,60.,30.92));
#2666=CARTESIAN_POINT('',(1.8,15.,30.92));
#2667=CARTESIAN_POINT('',(1.8,60.,0.));
#2668=CARTESIAN_POINT('Origin',(1.555,30.,30.92));
#2669=CARTESIAN_POINT('',(0.7775,0.,30.92));
#2670=CARTESIAN_POINT('Origin',(1.555,30.,30.92));
#2671=CARTESIAN_POINT('',(1.6775,60.,30.92));
#2672=CARTESIAN_POINT('Origin',(1.555,30.,29.08));
#2673=CARTESIAN_POINT('',(1.8,0.,29.08));
#2674=CARTESIAN_POINT('',(0.7775,0.,29.08));
#2675=CARTESIAN_POINT('',(1.8,15.,29.08));
#2676=CARTESIAN_POINT('Origin',(1.555,30.,29.08));
#2677=CARTESIAN_POINT('',(1.8,60.,29.08));
#2678=CARTESIAN_POINT('',(1.8,15.,29.08));
#2679=CARTESIAN_POINT('',(1.6775,60.,29.08));
#2680=CARTESIAN_POINT('Origin',(1.8,0.,0.));
#2681=CARTESIAN_POINT('',(1.8,0.,1.82));
#2682=CARTESIAN_POINT('',(1.8,0.,0.));
#2683=CARTESIAN_POINT('',(1.8,15.,1.82));
#2684=CARTESIAN_POINT('Origin',(1.8,0.,0.));
#2685=CARTESIAN_POINT('',(1.8,60.,1.82));
#2686=CARTESIAN_POINT('',(1.8,15.,1.82));
#2687=CARTESIAN_POINT('',(1.8,60.,0.));
#2688=CARTESIAN_POINT('Origin',(1.555,30.,1.82));
#2689=CARTESIAN_POINT('',(0.7775,0.,1.82));
#2690=CARTESIAN_POINT('Origin',(1.555,30.,1.82));
#2691=CARTESIAN_POINT('',(1.6775,60.,1.82));
#2692=CARTESIAN_POINT('Origin',(1.8,60.,0.));
#2693=CARTESIAN_POINT('',(0.,60.,0.));
#2694=CARTESIAN_POINT('',(1.8,60.,0.));
#2695=CARTESIAN_POINT('',(0.,60.,180.));
#2696=CARTESIAN_POINT('',(0.,60.,0.));
#2697=CARTESIAN_POINT('',(1.8,60.,180.));
#2698=CARTESIAN_POINT('Origin',(0.9,30.,0.));
#2699=CARTESIAN_POINT('',(0.,0.,0.));
#2700=CARTESIAN_POINT('',(0.,0.,0.));
#2701=CARTESIAN_POINT('',(0.,60.,0.));
#2702=CARTESIAN_POINT('Origin',(0.,0.,0.));
#2703=CARTESIAN_POINT('',(0.,0.,180.));
#2704=CARTESIAN_POINT('',(0.,0.,180.));
#2705=CARTESIAN_POINT('',(0.,0.,0.));
#2706=CARTESIAN_POINT('Origin',(0.,60.,0.));
#2707=CARTESIAN_POINT('',(0.,60.,180.));
#2708=CARTESIAN_POINT('Origin',(0.9,30.,180.));
#2709=CARTESIAN_POINT('',(0.,0.,0.));
#2710=CARTESIAN_POINT('Origin',(0.,58.18,1.3));
#2711=CARTESIAN_POINT('',(57.36,58.18,1.8));
#2712=CARTESIAN_POINT('',(0.,58.18,1.8));
#2713=CARTESIAN_POINT('',(14.34,58.18,1.8));
#2714=CARTESIAN_POINT('',(57.36,58.18,1.3));
#2715=CARTESIAN_POINT('',(57.36,58.18,0.65));
#2716=CARTESIAN_POINT('',(0.,58.18,1.3));
#2717=CARTESIAN_POINT('',(0.,58.18,1.3));
#2718=CARTESIAN_POINT('',(0.,58.18,0.65));
#2719=CARTESIAN_POINT('Origin',(57.36,58.82,1.3));
#2720=CARTESIAN_POINT('',(0.,58.82,1.8));
#2721=CARTESIAN_POINT('',(57.36,58.82,1.8));
#2722=CARTESIAN_POINT('',(43.02,58.82,1.8));
#2723=CARTESIAN_POINT('',(0.,58.82,1.3));
#2724=CARTESIAN_POINT('',(0.,58.82,0.65));
#2725=CARTESIAN_POINT('',(57.36,58.82,1.3));
#2726=CARTESIAN_POINT('',(57.36,58.82,1.3));
#2727=CARTESIAN_POINT('',(57.36,58.82,0.65));
#2728=CARTESIAN_POINT('Origin',(28.68,58.5,1.3));
#2729=CARTESIAN_POINT('',(0.,59.25,1.3));
#2730=CARTESIAN_POINT('',(57.36,29.25,1.3));
#2731=CARTESIAN_POINT('Origin',(57.36,0.,0.));
#2732=CARTESIAN_POINT('',(57.36,0.,1.8));
#2733=CARTESIAN_POINT('',(57.36,0.,1.8));
#2734=CARTESIAN_POINT('',(57.36,0.,0.));
#2735=CARTESIAN_POINT('',(57.36,0.,0.));
#2736=CARTESIAN_POINT('',(57.36,60.,0.));
#2737=CARTESIAN_POINT('',(57.36,0.,0.));
#2738=CARTESIAN_POINT('',(57.36,60.,1.8));
#2739=CARTESIAN_POINT('',(57.36,60.,0.));
#2740=CARTESIAN_POINT('',(57.36,0.,1.8));
#2741=CARTESIAN_POINT('Origin',(28.68,30.,1.8));
#2742=CARTESIAN_POINT('',(0.,0.,1.8));
#2743=CARTESIAN_POINT('',(0.,60.,1.8));
#2744=CARTESIAN_POINT('',(0.,0.,1.8));
#2745=CARTESIAN_POINT('Origin',(57.36,60.,0.));
#2746=CARTESIAN_POINT('',(0.,60.,0.));
#2747=CARTESIAN_POINT('',(57.36,60.,0.));
#2748=CARTESIAN_POINT('',(0.,60.,1.8));
#2749=CARTESIAN_POINT('',(0.,60.,0.));
#2750=CARTESIAN_POINT('',(57.36,60.,1.8));
#2751=CARTESIAN_POINT('Origin',(0.,0.,0.));
#2752=CARTESIAN_POINT('',(0.,0.,0.));
#2753=CARTESIAN_POINT('',(0.,0.,0.));
#2754=CARTESIAN_POINT('',(0.,0.,0.));
#2755=CARTESIAN_POINT('Origin',(0.,60.,0.));
#2756=CARTESIAN_POINT('',(0.,60.,1.8));
#2757=CARTESIAN_POINT('',(0.,60.,0.));
#2758=CARTESIAN_POINT('Origin',(28.68,30.,1.8));
#2759=CARTESIAN_POINT('Origin',(28.68,30.,0.));
#2760=CARTESIAN_POINT('',(0.,0.,0.));
#2761=CARTESIAN_POINT('Origin',(57.36,0.6,0.));
#2762=CARTESIAN_POINT('',(57.36,0.6,0.));
#2763=CARTESIAN_POINT('',(0.,0.6,0.));
#2764=CARTESIAN_POINT('',(57.36,0.6,0.));
#2765=CARTESIAN_POINT('',(0.,0.6,177.36));
#2766=CARTESIAN_POINT('',(0.,0.6,0.));
#2767=CARTESIAN_POINT('',(57.36,0.6,177.36));
#2768=CARTESIAN_POINT('',(57.36,0.6,177.36));
#2769=CARTESIAN_POINT('',(57.36,0.6,0.));
#2770=CARTESIAN_POINT('Origin',(57.36,0.,0.));
#2771=CARTESIAN_POINT('',(57.36,0.,0.));
#2772=CARTESIAN_POINT('',(57.36,0.,0.));
#2773=CARTESIAN_POINT('',(57.36,0.,177.36));
#2774=CARTESIAN_POINT('',(57.36,0.,177.36));
#2775=CARTESIAN_POINT('',(57.36,0.,0.));
#2776=CARTESIAN_POINT('Origin',(0.,0.,0.));
#2777=CARTESIAN_POINT('',(0.,0.,0.));
#2778=CARTESIAN_POINT('',(0.,0.,0.));
#2779=CARTESIAN_POINT('',(0.,0.,177.36));
#2780=CARTESIAN_POINT('',(0.,0.,177.36));
#2781=CARTESIAN_POINT('',(0.,0.,0.));
#2782=CARTESIAN_POINT('Origin',(0.,0.6,0.));
#2783=CARTESIAN_POINT('',(0.,0.6,0.));
#2784=CARTESIAN_POINT('',(0.,0.6,177.36));
#2785=CARTESIAN_POINT('Origin',(28.68,0.3,177.36));
#2786=CARTESIAN_POINT('Origin',(28.68,0.3,0.));
#2787=CARTESIAN_POINT('',(0.,0.,0.));
#2788=CARTESIAN_POINT('Origin',(57.36,57.6,0.));
#2789=CARTESIAN_POINT('',(57.36,57.6,0.));
#2790=CARTESIAN_POINT('',(0.,57.6,0.));
#2791=CARTESIAN_POINT('',(57.36,57.6,0.));
#2792=CARTESIAN_POINT('',(0.,57.6,1.8));
#2793=CARTESIAN_POINT('',(0.,57.6,0.));
#2794=CARTESIAN_POINT('',(57.36,57.6,1.8));
#2795=CARTESIAN_POINT('',(57.36,57.6,1.8));
#2796=CARTESIAN_POINT('',(57.36,57.6,0.));
#2797=CARTESIAN_POINT('Origin',(57.36,0.6,0.));
#2798=CARTESIAN_POINT('',(57.36,0.6,0.));
#2799=CARTESIAN_POINT('',(57.36,0.6,0.));
#2800=CARTESIAN_POINT('',(57.36,0.600000000000001,1.8));
#2801=CARTESIAN_POINT('',(57.36,0.6,1.8));
#2802=CARTESIAN_POINT('',(57.36,0.6,0.));
#2803=CARTESIAN_POINT('Origin',(0.,0.6,0.));
#2804=CARTESIAN_POINT('',(0.,0.600000000000001,0.));
#2805=CARTESIAN_POINT('',(0.,0.6,0.));
#2806=CARTESIAN_POINT('',(0.,0.600000000000001,1.8));
#2807=CARTESIAN_POINT('',(0.,0.6,1.8));
#2808=CARTESIAN_POINT('',(0.,0.600000000000001,0.));
#2809=CARTESIAN_POINT('Origin',(0.,57.6,0.));
#2810=CARTESIAN_POINT('',(0.,57.6,0.));
#2811=CARTESIAN_POINT('',(0.,57.6,1.8));
#2812=CARTESIAN_POINT('Origin',(28.68,29.1,1.8));
#2813=CARTESIAN_POINT('Origin',(28.68,29.1,0.));
#2814=CARTESIAN_POINT('',(0.,0.,0.));
#2815=CARTESIAN_POINT('Origin',(0.,0.,0.));
#2816=CARTESIAN_POINT('',(-0.4,-4.89858719658941E-17,2.8));
#2817=CARTESIAN_POINT('Origin',(0.,0.,2.8));
#2818=CARTESIAN_POINT('',(-0.4,-4.89858719658941E-17,0.));
#2819=CARTESIAN_POINT('',(-0.4,-4.89858719658941E-17,0.));
#2820=CARTESIAN_POINT('Origin',(0.,0.,0.));
#2821=CARTESIAN_POINT('Origin',(0.,0.,2.8));
#2822=CARTESIAN_POINT('Origin',(0.,0.,0.));
#2823=CARTESIAN_POINT('',(0.,0.,0.));
#2824=CARTESIAN_POINT('',(1.32,0.,0.));
#2825=CARTESIAN_POINT('',(1.32,58.2,1.32));
#2826=CARTESIAN_POINT('',(1.32,0.,29.1));
#2827=CARTESIAN_POINT('',(58.6,9.,64.));
#2828=CARTESIAN_POINT('',(60.,0.,180.));
#2829=CARTESIAN_POINT('',(58.68,0.,180.));
#2830=CARTESIAN_POINT('',(1.32,0.,59.1));
#2831=CARTESIAN_POINT('',(1.32,0.,89.1));
#2832=CARTESIAN_POINT('',(1.32,0.,119.1));
#2833=CARTESIAN_POINT('',(1.32,0.,149.1));
#2834=CARTESIAN_POINT('',(60.,0.,0.));
#2835=CARTESIAN_POINT('',(120.,0.,180.));
#2836=CARTESIAN_POINT('',(61.32,0.,0.));
#2837=CARTESIAN_POINT('',(118.68,0.,180.));
#2838=CARTESIAN_POINT('',(61.32,58.2,1.32));
#2839=CARTESIAN_POINT('',(61.32,0.,29.1));
#2840=CARTESIAN_POINT('',(61.32,0.,59.1));
#2841=CARTESIAN_POINT('',(61.32,0.,89.1));
#2842=CARTESIAN_POINT('',(61.32,0.,119.1));
#2843=CARTESIAN_POINT('',(61.32,0.,149.1));
#2844=CARTESIAN_POINT('',(58.6,9.,116.));
#2845=CARTESIAN_POINT('',(58.6,51.,64.));
#2846=CARTESIAN_POINT('',(58.6,51.,116.));
#2847=UNCERTAINTY_MEASURE_WITH_UNIT(LENGTH_MEASURE(0.001),#2861,
'DISTANCE_ACCURACY_VALUE',
'Maximum model space distance between geometric entities at asserted c
onnectivities');
#2848=UNCERTAINTY_MEASURE_WITH_UNIT(LENGTH_MEASURE(0.001),#2861,
'DISTANCE_ACCURACY_VALUE',
'Maximum model space distance between geometric entities at asserted c
onnectivities');
#2849=UNCERTAINTY_MEASURE_WITH_UNIT(LENGTH_MEASURE(0.001),#2861,
'DISTANCE_ACCURACY_VALUE',
'Maximum model space distance between geometric entities at asserted c
onnectivities');
#2850=UNCERTAINTY_MEASURE_WITH_UNIT(LENGTH_MEASURE(0.001),#2861,
'DISTANCE_ACCURACY_VALUE',
'Maximum model space distance between geometric entities at asserted c
onnectivities');
#2851=UNCERTAINTY_MEASURE_WITH_UNIT(LENGTH_MEASURE(0.001),#2861,
'DISTANCE_ACCURACY_VALUE',
'Maximum model space distance between geometric entities at asserted c
onnectivities');
#2852=UNCERTAINTY_MEASURE_WITH_UNIT(LENGTH_MEASURE(0.001),#2861,
'DISTANCE_ACCURACY_VALUE',
'Maximum model space distance between geometric entities at asserted c
onnectivities');
#2853=UNCERTAINTY_MEASURE_WITH_UNIT(LENGTH_MEASURE(0.001),#2861,
'DISTANCE_ACCURACY_VALUE',
'Maximum model space distance between geometric entities at asserted c
onnectivities');
#2854=(
GEOMETRIC_REPRESENTATION_CONTEXT(3)
GLOBAL_UNCERTAINTY_ASSIGNED_CONTEXT((#2847))
GLOBAL_UNIT_ASSIGNED_CONTEXT((#2861,#2863,#2864))
REPRESENTATION_CONTEXT('','3D')
);
#2855=(
GEOMETRIC_REPRESENTATION_CONTEXT(3)
GLOBAL_UNCERTAINTY_ASSIGNED_CONTEXT((#2848))
GLOBAL_UNIT_ASSIGNED_CONTEXT((#2861,#2863,#2864))
REPRESENTATION_CONTEXT('','3D')
);
#2856=(
GEOMETRIC_REPRESENTATION_CONTEXT(3)
GLOBAL_UNCERTAINTY_ASSIGNED_CONTEXT((#2849))
GLOBAL_UNIT_ASSIGNED_CONTEXT((#2861,#2863,#2864))
REPRESENTATION_CONTEXT('','3D')
);
#2857=(
GEOMETRIC_REPRESENTATION_CONTEXT(3)
GLOBAL_UNCERTAINTY_ASSIGNED_CONTEXT((#2850))
GLOBAL_UNIT_ASSIGNED_CONTEXT((#2861,#2863,#2864))
REPRESENTATION_CONTEXT('','3D')
);
#2858=(
GEOMETRIC_REPRESENTATION_CONTEXT(3)
GLOBAL_UNCERTAINTY_ASSIGNED_CONTEXT((#2851))
GLOBAL_UNIT_ASSIGNED_CONTEXT((#2861,#2863,#2864))
REPRESENTATION_CONTEXT('','3D')
);
#2859=(
GEOMETRIC_REPRESENTATION_CONTEXT(3)
GLOBAL_UNCERTAINTY_ASSIGNED_CONTEXT((#2852))
GLOBAL_UNIT_ASSIGNED_CONTEXT((#2861,#2863,#2864))
REPRESENTATION_CONTEXT('','3D')
);
#2860=(
GEOMETRIC_REPRESENTATION_CONTEXT(3)
GLOBAL_UNCERTAINTY_ASSIGNED_CONTEXT((#2853))
GLOBAL_UNIT_ASSIGNED_CONTEXT((#2861,#2863,#2864))
REPRESENTATION_CONTEXT('','3D')
);
#2861=(
LENGTH_UNIT()
NAMED_UNIT(*)
SI_UNIT(.CENTI.,.METRE.)
);
#2862=(
LENGTH_UNIT()
NAMED_UNIT(*)
SI_UNIT($,.METRE.)
);
#2863=(
NAMED_UNIT(*)
PLANE_ANGLE_UNIT()
SI_UNIT($,.RADIAN.)
);
#2864=(
NAMED_UNIT(*)
SI_UNIT($,.STERADIAN.)
SOLID_ANGLE_UNIT()
);
#2865=SHAPE_DEFINITION_REPRESENTATION(#2871,#2901);
#2866=SHAPE_DEFINITION_REPRESENTATION(#2872,#2902);
#2867=SHAPE_DEFINITION_REPRESENTATION(#2873,#2903);
#2868=SHAPE_DEFINITION_REPRESENTATION(#2874,#2904);
#2869=SHAPE_DEFINITION_REPRESENTATION(#2875,#2905);
#2870=SHAPE_DEFINITION_REPRESENTATION(#2876,#2906);
#2871=PRODUCT_DEFINITION_SHAPE('',$,#2908);
#2872=PRODUCT_DEFINITION_SHAPE('',$,#2909);
#2873=PRODUCT_DEFINITION_SHAPE('',$,#2910);
#2874=PRODUCT_DEFINITION_SHAPE('',$,#2911);
#2875=PRODUCT_DEFINITION_SHAPE('',$,#2912);
#2876=PRODUCT_DEFINITION_SHAPE('',$,#2913);
#2877=PRODUCT_DEFINITION_SHAPE($,$,#83);
#2878=PRODUCT_DEFINITION_SHAPE($,$,#84);
#2879=PRODUCT_DEFINITION_SHAPE($,$,#85);
#2880=PRODUCT_DEFINITION_SHAPE($,$,#86);
#2881=PRODUCT_DEFINITION_SHAPE($,$,#87);
#2882=PRODUCT_DEFINITION_SHAPE($,$,#88);
#2883=PRODUCT_DEFINITION_SHAPE($,$,#89);
#2884=PRODUCT_DEFINITION_SHAPE($,$,#90);
#2885=PRODUCT_DEFINITION_SHAPE($,$,#91);
#2886=PRODUCT_DEFINITION_SHAPE($,$,#92);
#2887=PRODUCT_DEFINITION_SHAPE($,$,#93);
#2888=PRODUCT_DEFINITION_SHAPE($,$,#94);
#2889=PRODUCT_DEFINITION_SHAPE($,$,#95);
#2890=PRODUCT_DEFINITION_SHAPE($,$,#96);
#2891=PRODUCT_DEFINITION_SHAPE($,$,#97);
#2892=PRODUCT_DEFINITION_SHAPE($,$,#98);
#2893=PRODUCT_DEFINITION_SHAPE($,$,#99);
#2894=PRODUCT_DEFINITION_SHAPE($,$,#100);
#2895=PRODUCT_DEFINITION_SHAPE($,$,#101);
#2896=PRODUCT_DEFINITION_SHAPE($,$,#102);
#2897=PRODUCT_DEFINITION_SHAPE($,$,#103);
#2898=PRODUCT_DEFINITION_SHAPE($,$,#104);
#2899=PRODUCT_DEFINITION_SHAPE($,$,#105);
#2900=PRODUCT_DEFINITION_SHAPE($,$,#106);
#2901=SHAPE_REPRESENTATION('',(#1775,#1878,#1879,#1880,#1881,#1882,#1883,
#1884,#1885,#1886,#1887,#1888,#1889,#1890,#1891,#1892,#1893,#1894,#1895,
#1896,#1897,#1898,#1899,#1900,#1901),#2854);
#2902=SHAPE_REPRESENTATION('',(#1776),#2855);
#2903=SHAPE_REPRESENTATION('',(#1847),#2856);
#2904=SHAPE_REPRESENTATION('',(#1858),#2857);
#2905=SHAPE_REPRESENTATION('',(#1865),#2858);
#2906=SHAPE_REPRESENTATION('',(#1872),#2859);
#2907=PRODUCT_DEFINITION_CONTEXT('part definition',#2927,'design');
#2908=PRODUCT_DEFINITION('TAS-023','TAS-023',#2914,#2907);
#2909=PRODUCT_DEFINITION('Universal side panel','Universal side panel',
#2915,#2907);
#2910=PRODUCT_DEFINITION('Horizontal closure panel',
'Horizontal closure panel',#2916,#2907);
#2911=PRODUCT_DEFINITION('Captured back panel','Captured back panel',#2917,
#2907);
#2912=PRODUCT_DEFINITION('Fixed shelf','Fixed shelf',#2918,#2907);
#2913=PRODUCT_DEFINITION('Bay coupling dowel','Bay coupling dowel',#2919,
#2907);
#2914=PRODUCT_DEFINITION_FORMATION('',$,#2929);
#2915=PRODUCT_DEFINITION_FORMATION('',$,#2930);
#2916=PRODUCT_DEFINITION_FORMATION('',$,#2931);
#2917=PRODUCT_DEFINITION_FORMATION('',$,#2932);
#2918=PRODUCT_DEFINITION_FORMATION('',$,#2933);
#2919=PRODUCT_DEFINITION_FORMATION('',$,#2934);
#2920=PRODUCT_RELATED_PRODUCT_CATEGORY('TAS-023','TAS-023',(#2929));
#2921=PRODUCT_RELATED_PRODUCT_CATEGORY('Universal side panel',
'Universal side panel',(#2930));
#2922=PRODUCT_RELATED_PRODUCT_CATEGORY('Horizontal closure panel',
'Horizontal closure panel',(#2931));
#2923=PRODUCT_RELATED_PRODUCT_CATEGORY('Captured back panel',
'Captured back panel',(#2932));
#2924=PRODUCT_RELATED_PRODUCT_CATEGORY('Fixed shelf','Fixed shelf',(#2933));
#2925=PRODUCT_RELATED_PRODUCT_CATEGORY('Bay coupling dowel',
'Bay coupling dowel',(#2934));
#2926=APPLICATION_PROTOCOL_DEFINITION('international standard',
'automotive_design',2009,#2927);
#2927=APPLICATION_CONTEXT(
'Core Data for Automotive Mechanical Design Process');
#2928=PRODUCT_CONTEXT('part definition',#2927,'mechanical');
#2929=PRODUCT('TAS-023','TAS-023',$,(#2928));
#2930=PRODUCT('Universal side panel','Universal side panel',$,(#2928));
#2931=PRODUCT('Horizontal closure panel','Horizontal closure panel',$,(#2928));
#2932=PRODUCT('Captured back panel','Captured back panel',$,(#2928));
#2933=PRODUCT('Fixed shelf','Fixed shelf',$,(#2928));
#2934=PRODUCT('Bay coupling dowel','Bay coupling dowel',$,(#2928));
#2935=PRESENTATION_STYLE_ASSIGNMENT((#2941));
#2936=PRESENTATION_STYLE_ASSIGNMENT((#2942));
#2937=PRESENTATION_STYLE_ASSIGNMENT((#2943));
#2938=PRESENTATION_STYLE_ASSIGNMENT((#2944));
#2939=PRESENTATION_STYLE_ASSIGNMENT((#2945));
#2940=PRESENTATION_STYLE_ASSIGNMENT((#2946));
#2941=SURFACE_STYLE_USAGE(.BOTH.,#2947);
#2942=SURFACE_STYLE_USAGE(.BOTH.,#2948);
#2943=SURFACE_STYLE_USAGE(.BOTH.,#2949);
#2944=SURFACE_STYLE_USAGE(.BOTH.,#2950);
#2945=SURFACE_STYLE_USAGE(.BOTH.,#2951);
#2946=SURFACE_STYLE_USAGE(.BOTH.,#2952);
#2947=SURFACE_SIDE_STYLE('',(#2953));
#2948=SURFACE_SIDE_STYLE('',(#2954));
#2949=SURFACE_SIDE_STYLE('',(#2955));
#2950=SURFACE_SIDE_STYLE('',(#2956));
#2951=SURFACE_SIDE_STYLE('',(#2957));
#2952=SURFACE_SIDE_STYLE('',(#2958));
#2953=SURFACE_STYLE_FILL_AREA(#2959);
#2954=SURFACE_STYLE_FILL_AREA(#2960);
#2955=SURFACE_STYLE_FILL_AREA(#2961);
#2956=SURFACE_STYLE_FILL_AREA(#2962);
#2957=SURFACE_STYLE_FILL_AREA(#2963);
#2958=SURFACE_STYLE_FILL_AREA(#2964);
#2959=FILL_AREA_STYLE('Steel - Satin',(#2965));
#2960=FILL_AREA_STYLE('Universal side panel finish',(#2966));
#2961=FILL_AREA_STYLE('Horizontal closure panel finish',(#2967));
#2962=FILL_AREA_STYLE('Captured back panel finish',(#2968));
#2963=FILL_AREA_STYLE('Fixed shelf finish',(#2969));
#2964=FILL_AREA_STYLE('Bay coupling dowel finish',(#2970));
#2965=FILL_AREA_STYLE_COLOUR('Steel - Satin',#2971);
#2966=FILL_AREA_STYLE_COLOUR('Universal side panel finish',#2972);
#2967=FILL_AREA_STYLE_COLOUR('Horizontal closure panel finish',#2973);
#2968=FILL_AREA_STYLE_COLOUR('Captured back panel finish',#2974);
#2969=FILL_AREA_STYLE_COLOUR('Fixed shelf finish',#2975);
#2970=FILL_AREA_STYLE_COLOUR('Bay coupling dowel finish',#2976);
#2971=COLOUR_RGB('Steel - Satin',0.627450980392157,0.627450980392157,0.627450980392157);
#2972=COLOUR_RGB('Universal side panel finish',0.0941176470588235,0.231372549019608,
0.431372549019608);
#2973=COLOUR_RGB('Horizontal closure panel finish',0.662745098039216,0.823529411764706,
0.917647058823529);
#2974=COLOUR_RGB('Captured back panel finish',0.607843137254902,0.647058823529412,
0.701960784313725);
#2975=COLOUR_RGB('Fixed shelf finish',0.274509803921569,0.6,0.8);
#2976=COLOUR_RGB('Bay coupling dowel finish',0.43921568627451,0.47843137254902,
0.52156862745098);
ENDSEC;
END-ISO-10303-21;
